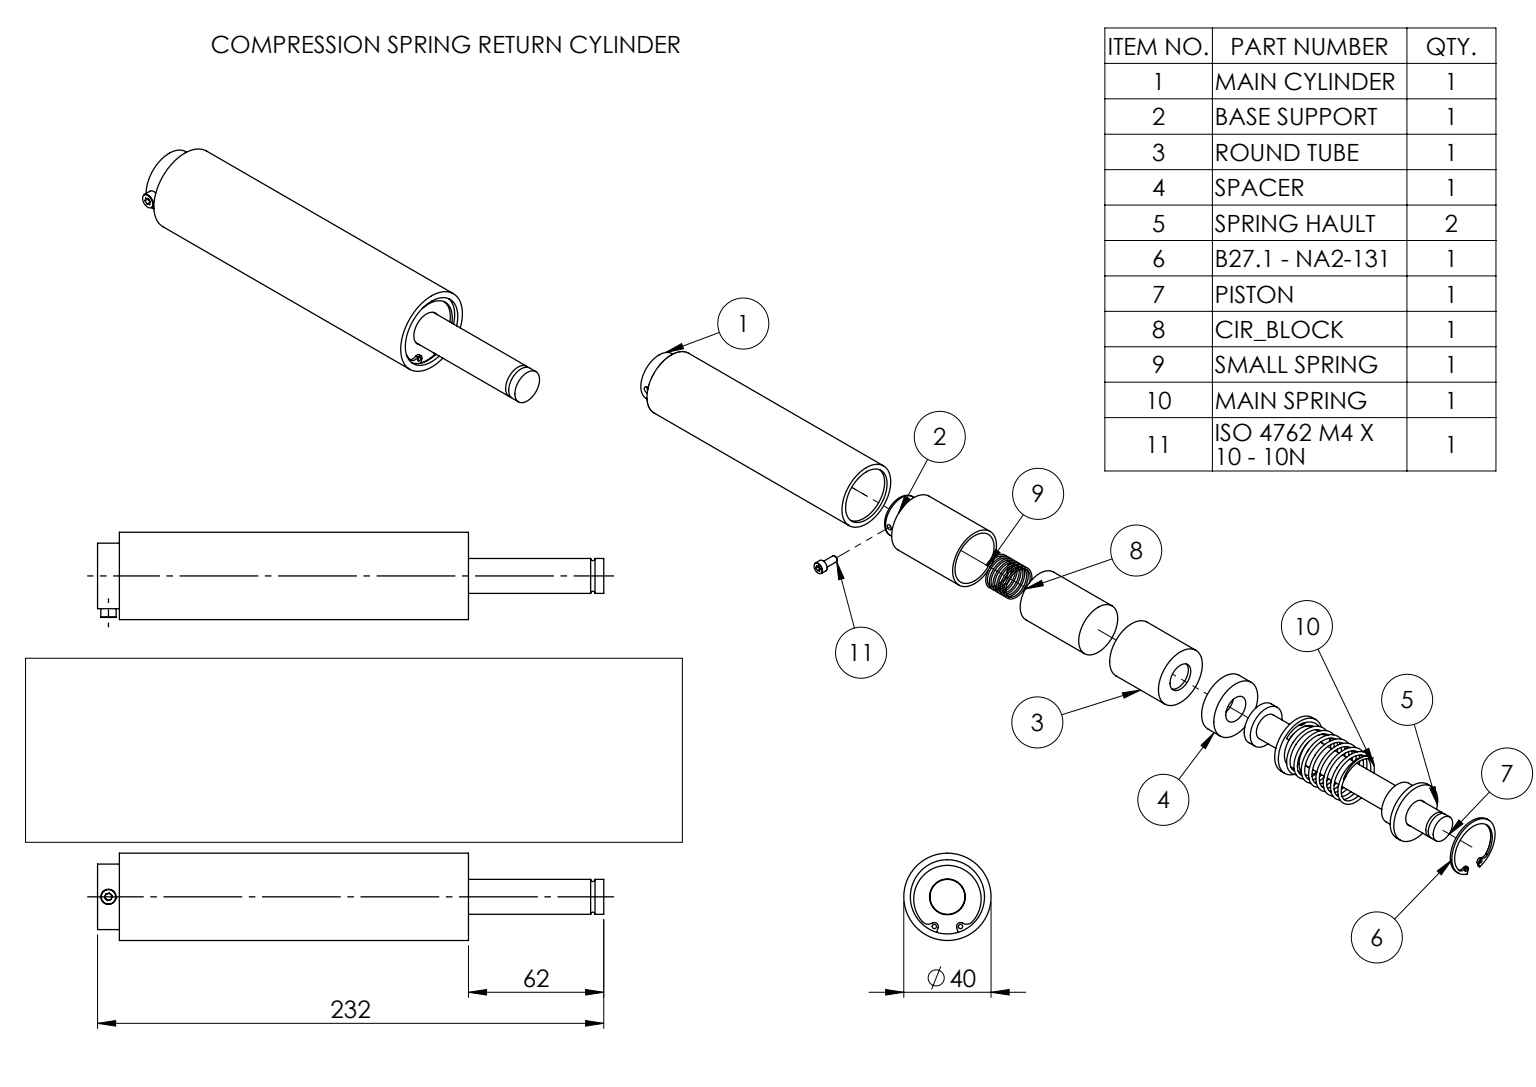
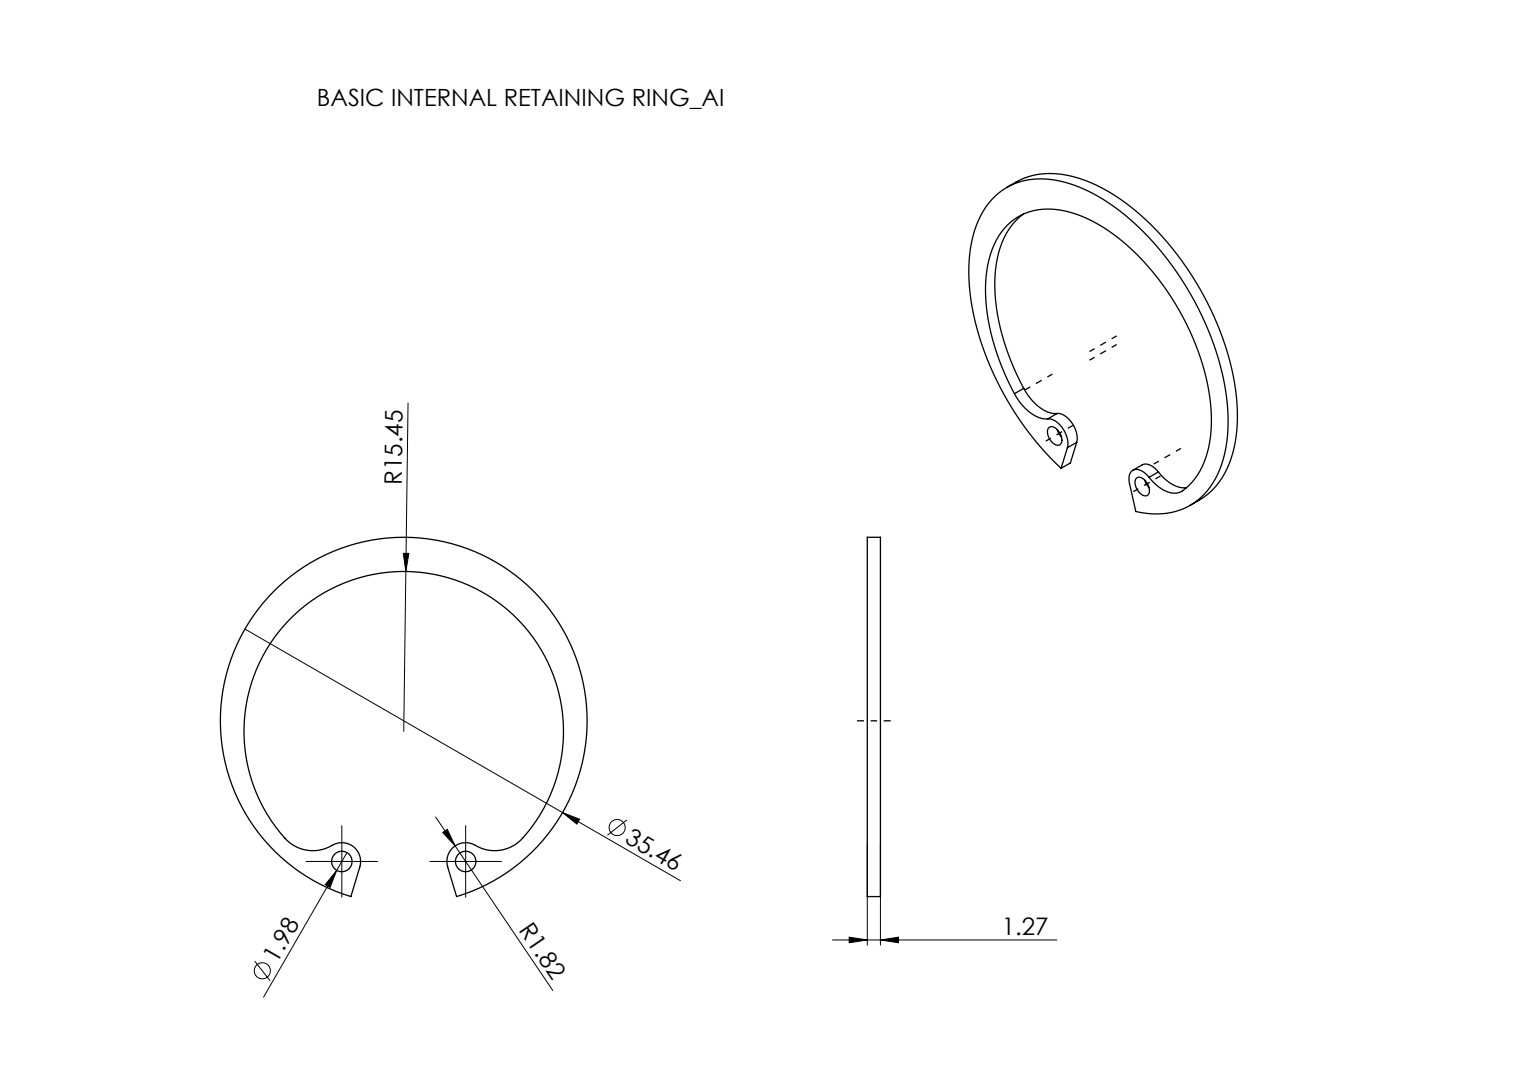
ISO-10303-21;
HEADER;
FILE_DESCRIPTION (('STEP AP214'),
    '1' );
FILE_NAME ('BR-105',
    '2026-10-08T13:22:57',
    ( '' ),
    ( '' ),
    'SwSTEP 2.0',
    'SolidWorks 2026',
    '' );
FILE_SCHEMA (( 'AUTOMOTIVE_DESIGN' ));
ENDSEC;

DATA;
#1 = CARTESIAN_POINT ( 'NONE',  ( -9.837026868206070418, 5.012215536711416952, 5.849999999999989875 ) ) ;
#2 = CARTESIAN_POINT ( 'NONE',  ( 8.512513224245308763, 13.54758718765259040, 13.28571428571429003 ) ) ;
#3 = EDGE_CURVE ( 'NONE', #2841, #2214, #7627, .T. ) ;
#4 = CARTESIAN_POINT ( 'NONE',  ( 0.000000000000000000, 0.000000000000000000, -1.270000000000007123 ) ) ;
#5 = CARTESIAN_POINT ( 'NONE',  ( -14.28433602490915000, 1.478298951650542481, 25.35310228751642470 ) ) ;
#6 = CARTESIAN_POINT ( 'NONE',  ( 9.377220287599001836, 4.724406229267489543, 5.901137918078571687 ) ) ;
#7 = CARTESIAN_POINT ( 'NONE',  ( 8.486213763410640709, 4.270415729527937465, 17.90113791807857524 ) ) ;
#8 = AXIS2_PLACEMENT_3D ( 'NONE', #6315, #4531, #6166 ) ;
#9 = AXIS2_PLACEMENT_3D ( 'NONE', #1726, #4047, #111 ) ;
#10 = LINE ( 'NONE', #4146, #4138 ) ;
#11 = CARTESIAN_POINT ( 'NONE',  ( -11.92174236212692051, -7.340858601238089420, 8.718326283912148256 ) ) ;
#12 = CARTESIAN_POINT ( 'NONE',  ( 13.17239914596754424, -4.743843029824685864, 18.57546914105500235 ) ) ;
#13 = EDGE_CURVE ( 'NONE', #5655, #2841, #6772, .T. ) ;
#14 = ORIENTED_EDGE ( 'NONE', *, *, #6088, .F. ) ;
#15 = CARTESIAN_POINT ( 'NONE',  ( 15.44746603149413922, 5.543385399275817527, 15.92453085894499409 ) ) ;
#16 = COLOUR_RGB ( '', 0.40784314, 0.44705882, 0.49803922) ;
#17 = DIRECTION ( 'NONE',  ( 0.000000000000000000, 0.000000000000000000, 1.000000000000000000 ) ) ;
#18 = AXIS2_PLACEMENT_3D ( 'NONE', #9607, #4018, #5606 ) ;
#19 = AXIS2_PLACEMENT_3D ( 'NONE', #2999, #9984, #6972 ) ;
#20 = CARTESIAN_POINT ( 'NONE',  ( 11.31370849898482334, -11.31370849898469366, 45.00000000000000711 ) ) ;
#21 = CARTESIAN_POINT ( 'NONE',  ( -170.0000000000000284, -1.448262861947153525E-15, 0.000000000000000000 ) ) ;
#22 = CARTESIAN_POINT ( 'NONE',  ( 15.44569104238500046, -1.018491042385001544, -1.270000000000007123 ) ) ;
#23 = CARTESIAN_POINT ( 'NONE',  ( -4.312909747525649706, -8.464561979789507973, 14.10000000000000142 ) ) ;
#24 = CARTESIAN_POINT ( 'NONE',  ( 4.534861676072320158, -8.900167166472098046, 4.650000000000026112 ) ) ;
#25 = CARTESIAN_POINT ( 'NONE',  ( -8.731428362939189114, 13.89598863503036341, 36.21428571428573662 ) ) ;
#26 = CARTESIAN_POINT ( 'NONE',  ( 2.000000000000001776, 0.000000000000000000, 0.000000000000000000 ) ) ;
#27 = LINE ( 'NONE', #8664, #6923 ) ;
#28 = CARTESIAN_POINT ( 'NONE',  ( -11.22385875690717327, 11.40355824106234550, 28.00404056962643651 ) ) ;
#29 = ORIENTED_EDGE ( 'NONE', *, *, #8994, .F. ) ;
#30 = CARTESIAN_POINT ( 'NONE',  ( -1.837501619626328297, 16.30827793483733856, 12.64285714285714235 ) ) ;
#31 = CARTESIAN_POINT ( 'NONE',  ( 0.000000000000000000, -6.162975822039154730E-30, 20.00000000000001776 ) ) ;
#32 = AXIS2_PLACEMENT_3D ( 'NONE', #6124, #2105, #1276 ) ;
#33 = CARTESIAN_POINT ( 'NONE',  ( 0.000000000000000000, 0.000000000000000000, 0.000000000000000000 ) ) ;
#34 = CARTESIAN_POINT ( 'NONE',  ( -7.458344646081709328, 7.390897758835804687, 9.998862081921425116 ) ) ;
#35 = CARTESIAN_POINT ( 'NONE',  ( -13.92619789766827054, -1.441234910513399470, 45.14689771248358596 ) ) ;
#36 = CARTESIAN_POINT ( 'NONE',  ( 8.512513224245308763, 13.54758718765259040, 19.28571428571428825 ) ) ;
#37 = CONTEXT_DEPENDENT_SHAPE_REPRESENTATION ( #2747, #7395 ) ;
#38 = CARTESIAN_POINT ( 'NONE',  ( -7.639999817571786700, 12.15899005565156266, 36.21428571428572951 ) ) ;
#39 = CARTESIAN_POINT ( 'NONE',  ( 9.809645194534072132, -9.989344678689256796, 31.00404056962644006 ) ) ;
#40 = CARTESIAN_POINT ( 'NONE',  ( -9.865911304835474738, -1.562606840307925848, 8.549999999999963407 ) ) ;
#41 = CARTESIAN_POINT ( 'NONE',  ( 5.012215536711511987, -9.837026868205999364, 13.65000000000003233 ) ) ;
#42 = ORIENTED_EDGE ( 'NONE', *, *, #8056, .T. ) ;
#43 = CARTESIAN_POINT ( 'NONE',  ( 1.441234910513245149, 13.92619789766829008, 50.85310228751642825 ) ) ;
#44 = ORIENTED_EDGE ( 'NONE', *, *, #5565, .F. ) ;
#45 = DIRECTION ( 'NONE',  ( 1.000000000000000000, 0.000000000000000000, 0.000000000000000000 ) ) ;
#46 = CARTESIAN_POINT ( 'NONE',  ( 11.60466159355861926, 11.60466159355874716, 13.50000000000000355 ) ) ;
#47 = CIRCLE ( 'NONE', #69, 13.00000000000001066 ) ;
#48 = CARTESIAN_POINT ( 'NONE',  ( -13.96533075980324234, 8.621071003556515677, 19.78167371608784819 ) ) ;
#49 = DIRECTION ( 'NONE',  ( -1.000000000000000000, 0.000000000000000000, -0.000000000000000000 ) ) ;
#50 = CARTESIAN_POINT ( 'NONE',  ( 10.90442828429183919, 1.727091770866679532, 1.049999999999966738 ) ) ;
#51 = CARTESIAN_POINT ( 'NONE',  ( 17.72919999999999874, 0.000000000000000000, -1.270000000000007123 ) ) ;
#52 = CIRCLE ( 'NONE', #2688, 13.00000000000000000 ) ;
#53 = FILL_AREA_STYLE_COLOUR ( '', #3926 ) ;
#54 = EDGE_LOOP ( 'NONE', ( #8916, #8035, #5862, #4936 ) ) ;
#55 = CARTESIAN_POINT ( 'NONE',  ( 4.766900247265192903, 9.355568503977902850, 12.59999999999999964 ) ) ;
#56 = CARTESIAN_POINT ( 'NONE',  ( 1.791431617652837316, 15.89939535829188877, 12.85714285714285943 ) ) ;
#57 = CARTESIAN_POINT ( 'NONE',  ( 0.000000000000000000, 1.773042676681366281, 0.000000000000000000 ) ) ;
#58 = SHAPE_REPRESENTATION ( 'BR-105', ( #5082, #2288, #1626, #7233, #8720, #5896, #6061, #2114, #799, #7563, #6712, #8058, #5576 ), #3109 ) ;
#59 = CARTESIAN_POINT ( 'NONE',  ( 1.441234910513245149, 13.92619789766829008, 26.85310228751642470 ) ) ;
#60 = CARTESIAN_POINT ( 'NONE',  ( 4.809394265263009061, 9.333916720356739916, 8.601137918078563871 ) ) ;
#61 = CARTESIAN_POINT ( 'NONE',  ( -9.873755945037078874, -1.513077731353019706, 10.55113791807857204 ) ) ;
#62 = CARTESIAN_POINT ( 'NONE',  ( -108.0000000000000284, 0.000000000000000000, 18.00000000000000000 ) ) ;
#63 = CARTESIAN_POINT ( 'NONE',  ( 13.17239914596754424, -4.743843029824685864, 12.57546914105500768 ) ) ;
#64 = CARTESIAN_POINT ( 'NONE',  ( -1.478298951650703019, 14.28433602490913579, 10.64689771248357886 ) ) ;
#65 = ORIENTED_EDGE ( 'NONE', *, *, #5817, .F. ) ;
#66 = DIRECTION ( 'NONE',  ( 1.000000000000000000, 4.755747939841215952E-17, -0.000000000000000000 ) ) ;
#67 = ADVANCED_BREP_SHAPE_REPRESENTATION ( '', ( #183, #3995 ), #2439 ) ;
#68 = CARTESIAN_POINT ( 'NONE',  ( 15.89939535829187278, 1.791431617653015174, 44.14285714285714590 ) ) ;
#69 = AXIS2_PLACEMENT_3D ( 'NONE', #6608, #9795, #2698 ) ;
#70 = DIRECTION ( 'NONE',  ( 0.000000000000000000, 0.000000000000000000, 1.000000000000000000 ) ) ;
#71 = FACE_OUTER_BOUND ( 'NONE', #2223, .T. ) ;
#72 = CARTESIAN_POINT ( 'NONE',  ( 9.865911304835474738, 1.562606840307950051, 19.04999999999997939 ) ) ;
#73 = CARTESIAN_POINT ( 'NONE',  ( 8.900167166472154889, -4.534861676072210912, 7.350000000000000533 ) ) ;
#74 = EDGE_CURVE ( 'NONE', #951, #9116, #2667, .T. ) ;
#75 = CARTESIAN_POINT ( 'NONE',  ( -163.1352118936811451, 1.079191317860220156, 12.95565487998667820 ) ) ;
#76 = DIRECTION ( 'NONE',  ( 0.000000000000000000, 8.191099868251446680E-34, 1.000000000000000000 ) ) ;
#77 = CARTESIAN_POINT ( 'NONE',  ( -5.543385399275643444, -15.44746603149420494, 38.07546914105502367 ) ) ;
#78 = ORIENTED_EDGE ( 'NONE', *, *, #9774, .F. ) ;
#79 = CARTESIAN_POINT ( 'NONE',  ( -13.54758718765249625, -8.512513224245459753, 34.71428571428571530 ) ) ;
#80 = CARTESIAN_POINT ( 'NONE',  ( 2.336471713481377055, 15.82515143223400145, 48.73000000000002530 ) ) ;
#81 = DIRECTION ( 'NONE',  ( -4.755747939841216568E-17, 1.000000000000000000, 0.000000000000000000 ) ) ;
#82 = SURFACE_STYLE_USAGE ( .BOTH. , #1640 ) ;
#83 = CARTESIAN_POINT ( 'NONE',  ( 4.724406229267374968, 9.377220287599055126, 13.59886208192140167 ) ) ;
#84 = CARTESIAN_POINT ( 'NONE',  ( 5.056896391392317724, -9.814260835640977731, 14.64886208192141659 ) ) ;
#85 = CARTESIAN_POINT ( 'NONE',  ( -1.693770420379220099, -13.89774397934251837, 43.86118342676930126 ) ) ;
#86 = CARTESIAN_POINT ( 'NONE',  ( 16.30827793483735633, -1.837501619626142890, 20.35714285714286476 ) ) ;
#87 = CARTESIAN_POINT ( 'NONE',  ( -4.742819248065500481, -13.55419868402813499, 34.07142857142857650 ) ) ;
#88 = CARTESIAN_POINT ( 'NONE',  ( -5.164528828830334817, 15.14410076328347543, -1.567388001802134223 ) ) ;
#89 = CARTESIAN_POINT ( 'NONE',  ( -14.26974319298268767, 1.607813917172874918, 5.357142857142856762 ) ) ;
#90 = CARTESIAN_POINT ( 'NONE',  ( -1.486127417882243895, 9.383039235653816590, 15.29999999999997939 ) ) ;
#91 = CARTESIAN_POINT ( 'NONE',  ( 1.727091770866550968, 10.90442828429186761, 18.44999999999999218 ) ) ;
#92 = ORIENTED_EDGE ( 'NONE', *, *, #7588, .T. ) ;
#93 = CARTESIAN_POINT ( 'NONE',  ( -11.85413878919593422, -7.448449071214776396, 4.714285714285712636 ) ) ;
#94 = VERTEX_POINT ( 'NONE', #2924 ) ;
#95 = DIRECTION ( 'NONE',  ( 0.000000000000000000, 0.000000000000000000, 1.000000000000000000 ) ) ;
#96 = CARTESIAN_POINT ( 'NONE',  ( -8.512513224245306986, -13.54758718765259218, 16.28571428571428470 ) ) ;
#97 = CARTESIAN_POINT ( 'NONE',  ( -16.32287076676382398, 1.707986654103809343, 43.35310228751642825 ) ) ;
#98 = CARTESIAN_POINT ( 'NONE',  ( -160.0000000000000284, 19.99999999999999289, 0.000000000000000000 ) ) ;
#99 = CARTESIAN_POINT ( 'NONE',  ( -7.806708723663830618, -7.806708723663906113, 8.250000000000028422 ) ) ;
#100 = EDGE_CURVE ( 'NONE', #8895, #4771, #529, .T. ) ;
#101 = CARTESIAN_POINT ( 'NONE',  ( 4.742819248065502258, 13.55419868402813499, 1.071428571428570065 ) ) ;
#102 =( LENGTH_UNIT ( ) NAMED_UNIT ( * ) SI_UNIT ( .MILLI., .METRE. ) );
#103 = EDGE_LOOP ( 'NONE', ( #4875, #2005 ) ) ;
#104 = CARTESIAN_POINT ( 'NONE',  ( -10.06191849875405531, -10.24623928997363542, 12.49595943037356349 ) ) ;
#105 = CARTESIAN_POINT ( 'NONE',  ( -5.012215536711508435, 9.837026868206029562, 9.150000000000002132 ) ) ;
#106 = CARTESIAN_POINT ( 'NONE',  ( -163.3500000000000796, 0.1091377801384209867, 13.00000000000000178 ) ) ;
#107 = CARTESIAN_POINT ( 'NONE',  ( 7.750357176954296712, -12.08964793087877787, 41.21024514465928235 ) ) ;
#108 = CARTESIAN_POINT ( 'NONE',  ( -10.91227292449344155, -1.677562661911748965, 4.551137918078585365 ) ) ;
#109 = CARTESIAN_POINT ( 'NONE',  ( 9.375578539472099848, -1.533232399699987702, 15.20113791807854575 ) ) ;
#110 = CIRCLE ( 'NONE', #5390, 0.2000000000000000944 ) ;
#111 = DIRECTION ( 'NONE',  ( 1.000000000000000000, 0.000000000000000000, 0.000000000000000000 ) ) ;
#112 = CARTESIAN_POINT ( 'NONE',  ( -7.556039541191334585, -11.78653521626503320, 2.289754855340722539 ) ) ;
#113 =( LENGTH_UNIT ( ) NAMED_UNIT ( * ) SI_UNIT ( .MILLI., .METRE. ) );
#114 = CARTESIAN_POINT ( 'NONE',  ( 7.556039541191335474, 11.78653521626503320, 11.28975485534071943 ) ) ;
#115 = ORIENTED_EDGE ( 'NONE', *, *, #1311, .F. ) ;
#117 = CARTESIAN_POINT ( 'NONE',  ( 0.2000000000000057288, 4.041334437186265510E-16, -3.299999999999999822 ) ) ;
#116 = STYLED_ITEM ( 'NONE', ( #9052 ), #3700 ) ;
#118 = CARTESIAN_POINT ( 'NONE',  ( 11.60466159355862104, 11.60466159355875071, 37.50000000000002842 ) ) ;
#119 = CYLINDRICAL_SURFACE ( 'NONE', #383, 0.9906000000000003691 ) ;
#120 = CARTESIAN_POINT ( 'NONE',  ( -167.0926989554971556, -0.5670040589733402747, 14.99151548021192148 ) ) ;
#121 = CARTESIAN_POINT ( 'NONE',  ( 1.562606840307832368, 9.865911304835503159, 18.44999999999999218 ) ) ;
#122 = CARTESIAN_POINT ( 'NONE',  ( 7.063212654743467489, 7.063212654743559860, 3.749999999999997335 ) ) ;
#123 = CARTESIAN_POINT ( 'NONE',  ( -166.9317395015584680, 0.9543248124665052456, 12.96558013998003922 ) ) ;
#124 = CARTESIAN_POINT ( 'NONE',  ( 16.29368510291089223, -1.967016585148476882, 30.36118342676929771 ) ) ;
#125 = CARTESIAN_POINT ( 'NONE',  ( 7.063212654743468377, 7.063212654743558083, 0.7499999999999762412 ) ) ;
#126 = CARTESIAN_POINT ( 'NONE',  ( -11.22385875690717327, 11.40355824106234550, 34.00404056962644006 ) ) ;
#127 = EDGE_LOOP ( 'NONE', ( #6964, #4432, #9166, #5764, #3012, #4282, #881, #9298, #4822, #5247, #5054, #1752, #8600 ) ) ;
#128 = CARTESIAN_POINT ( 'NONE',  ( 8.731428362939190890, -13.89598863503036164, 33.21428571428571530 ) ) ;
#129 = CARTESIAN_POINT ( 'NONE',  ( 2.000000000000001776, 0.8865213383406900238, 1.535499999999967446 ) ) ;
#130 = CARTESIAN_POINT ( 'NONE',  ( 11.60466159355862104, 11.60466159355875071, 1.500000000000003553 ) ) ;
#131 = SURFACE_STYLE_FILL_AREA ( #8771 ) ;
#132 = ADVANCED_FACE ( 'NONE', ( #2160 ), #9918, .F. ) ;
#133 =( NAMED_UNIT ( * ) PLANE_ANGLE_UNIT ( ) SI_UNIT ( $, .RADIAN. ) );
#134 = CARTESIAN_POINT ( 'NONE',  ( -8.442910196168309511, -4.355403765523546689, 6.398862081921404155 ) ) ;
#135 = CARTESIAN_POINT ( 'NONE',  ( -5.056896391392315948, 9.814260835640997271, 16.14886208192145389 ) ) ;
#136 = CARTESIAN_POINT ( 'NONE',  ( 5.164528828830335705, -15.14410076328347543, 1.432611998197868219 ) ) ;
#137 = CARTESIAN_POINT ( 'NONE',  ( -1.791431617652833763, -15.89939535829188877, 21.85714285714286120 ) ) ;
#138 = CARTESIAN_POINT ( 'NONE',  ( -11.85413878919593422, -7.448449071214776396, 34.71428571428571530 ) ) ;
#139 = CARTESIAN_POINT ( 'NONE',  ( -9.809645194534070356, 9.989344678689256796, 46.00404056962644006 ) ) ;
#140 = CARTESIAN_POINT ( 'NONE',  ( -7.639999817571787588, 12.15899005565156266, 12.21428571428571885 ) ) ;
#141 = CARTESIAN_POINT ( 'NONE',  ( 1.562606840307832146, 9.865911304835508489, 15.44999999999997797 ) ) ;
#142 = CARTESIAN_POINT ( 'NONE',  ( -9.333916720356675967, -4.809394265263095214, 12.39886208192140948 ) ) ;
#143 = ORIENTED_EDGE ( 'NONE', *, *, #7111, .T. ) ;
#144 = CARTESIAN_POINT ( 'NONE',  ( -11.78653521626494793, -7.556039541191465148, 48.71024514465926814 ) ) ;
#145 = EDGE_LOOP ( 'NONE', ( #8443, #9716, #3991, #7695 ) ) ;
#146 = CARTESIAN_POINT ( 'NONE',  ( 0.000000000000000000, 0.8865213383407039016, -1.535500000000022958 ) ) ;
#147 = MANIFOLD_SOLID_BREP ( 'Revolve1', #1849 ) ;
#148 = CARTESIAN_POINT ( 'NONE',  ( 1.791431617652837316, 15.89939535829188877, 18.85714285714285765 ) ) ;
#149 = CARTESIAN_POINT ( 'NONE',  ( -15.14410076328353227, 5.164528828830164287, 31.56738800180213644 ) ) ;
#150 = CARTESIAN_POINT ( 'NONE',  ( -4.766900247265192014, -9.355568503977867323, 8.099999999999996092 ) ) ;
#151 = CARTESIAN_POINT ( 'NONE',  ( -4.766900247265192014, -9.355568503977867323, 8.099999999999996092 ) ) ;
#152 = FACE_BOUND ( 'NONE', #612, .T. ) ;
#153 = FILL_AREA_STYLE ('',( #53 ) ) ;
#154 = ORIENTED_EDGE ( 'NONE', *, *, #7460, .T. ) ;
#155 = CARTESIAN_POINT ( 'NONE',  ( -1.441234910513241818, -13.92619789766829008, 11.85310228751642470 ) ) ;
#156 = CARTESIAN_POINT ( 'NONE',  ( -5.012215536711508435, 9.837026868206020680, 18.15000000000000924 ) ) ;
#157 = CARTESIAN_POINT ( 'NONE',  ( -58.00000000000002842, 7.703719777548943412E-30, -1.059261469412979719E-30 ) ) ;
#158 = CARTESIAN_POINT ( 'NONE',  ( 7.340858601237956194, 11.92174236212700045, 45.28167371608785174 ) ) ;
#159 = CARTESIAN_POINT ( 'NONE',  ( -4.967534682030703586, 9.859792900771061852, 17.15113791807853616 ) ) ;
#160 = CARTESIAN_POINT ( 'NONE',  ( 4.490180821391514421, -8.922933199037132113, 12.65113791807859123 ) ) ;
#161 = EDGE_CURVE ( 'NONE', #3385, #4901, #5306, .T. ) ;
#162 = DIRECTION ( 'NONE',  ( 1.000000000000000000, 0.000000000000000000, 0.000000000000000000 ) ) ;
#163 = CARTESIAN_POINT ( 'NONE',  ( 4.865839792409144771, 13.51115193377589740, 17.07546914105500591 ) ) ;
#164 = AXIS2_PLACEMENT_3D ( 'NONE', #7046, #7979, #7201 ) ;
#165 = CARTESIAN_POINT ( 'NONE',  ( -11.92174236212692051, -7.340858601238089420, 8.718326283912148256 ) ) ;
#166 = VERTEX_POINT ( 'NONE', #3235 ) ;
#167 = LINE ( 'NONE', #8073, #9856 ) ;
#168 = CARTESIAN_POINT ( 'NONE',  ( -5.404401153735176599, 15.06016580658422477, 14.42453085894499232 ) ) ;
#169 = CYLINDRICAL_SURFACE ( 'NONE', #4836, 18.00000000000002132 ) ;
#170 = CARTESIAN_POINT ( 'NONE',  ( -165.9524913265358350, -1.932636693197999911, 14.87507538773749438 ) ) ;
#171 = CIRCLE ( 'NONE', #2486, 11.00000000000000355 ) ;
#172 = TOROIDAL_SURFACE ( 'NONE', #9093, 2.200000000000001066, 0.2000000000000000111 ) ;
#173 = CARTESIAN_POINT ( 'NONE',  ( -1.439022436064386845, 9.390499931835535108, 8.301137918078554279 ) ) ;
#174 = CARTESIAN_POINT ( 'NONE',  ( 1.486127417882244783, -9.383039235653782839, 7.800000000000029132 ) ) ;
#175 = CARTESIAN_POINT ( 'NONE',  ( -166.3219090446497432, 1.718560695228406932, 12.88744630017030168 ) ) ;
#176 = CARTESIAN_POINT ( 'NONE',  ( 8.621071003556677326, -13.96533075980314287, 31.21832628391215536 ) ) ;
#177 = CARTESIAN_POINT ( 'NONE',  ( -4.312909747525649706, -8.464561979789507973, 2.099999999999990763 ) ) ;
#178 = ADVANCED_FACE ( 'NONE', ( #1639 ), #6426, .T. ) ;
#179 = CARTESIAN_POINT ( 'NONE',  ( 8.620103694221997515, 13.47998361472160767, 29.28975485534071765 ) ) ;
#180 = CIRCLE ( 'NONE', #1825, 18.00000000000002132 ) ;
#181 = CIRCLE ( 'NONE', #5941, 18.00000000000000355 ) ;
#182 = ORIENTED_EDGE ( 'NONE', *, *, #837, .T. ) ;
#183 = MANIFOLD_SOLID_BREP ( 'Hex', #8118 ) ;
#184 = CARTESIAN_POINT ( 'NONE',  ( -15.89939535829186923, -1.791431617653016062, 29.14285714285714235 ) ) ;
#185 = CARTESIAN_POINT ( 'NONE',  ( -1.732852372895761661, 14.17511762181074353, 2.529641460854714575E-15 ) ) ;
#186 = CARTESIAN_POINT ( 'NONE',  ( -5.420364854931999155, -15.49051278174644253, 22.07142857142858006 ) ) ;
#187 =( NAMED_UNIT ( * ) PLANE_ANGLE_UNIT ( ) SI_UNIT ( $, .RADIAN. ) );
#188 = CARTESIAN_POINT ( 'NONE',  ( 5.986002070941135678, -13.58603705635637304, -1.270000000000007123 ) ) ;
#189 = AXIS2_PLACEMENT_3D ( 'NONE', #6209, #7825, #5544 ) ;
#190 = CARTESIAN_POINT ( 'NONE',  ( -9.390499931835536884, 1.439022436064298249, 6.698862081921455491 ) ) ;
#191 = CARTESIAN_POINT ( 'NONE',  ( -1.533232399700100057, 9.375578539472094519, 1.298862081921425604 ) ) ;
#192 =( GEOMETRIC_REPRESENTATION_CONTEXT ( 3 ) GLOBAL_UNCERTAINTY_ASSIGNED_CONTEXT ( ( #920 ) ) GLOBAL_UNIT_ASSIGNED_CONTEXT ( ( #9393, #2545, #4632 ) ) REPRESENTATION_CONTEXT ( 'NONE', 'WORKASPACE' ) );
#193 = UNCERTAINTY_MEASURE_WITH_UNIT (LENGTH_MEASURE( 1.000000000000000082E-05 ), #7498, 'distance_accuracy_value', 'NONE');
#194 = CARTESIAN_POINT ( 'NONE',  ( 12.08964793087886314, -7.750357176954162597, 42.78975485534072476 ) ) ;
#195 = CARTESIAN_POINT ( 'NONE',  ( 8.731428362939190890, -13.89598863503036164, 9.214285714285717077 ) ) ;
#196 = DIRECTION ( 'NONE',  ( 1.000000000000000000, 0.000000000000000000, 0.000000000000000000 ) ) ;
#197 = CARTESIAN_POINT ( 'NONE',  ( 4.503970704919991519, -13.25633410266674517, 43.43261199819787066 ) ) ;
#198 = CARTESIAN_POINT ( 'NONE',  ( -1.567502665446231180, -13.91197093850540334, 9.857142857142855874 ) ) ;
#199 = CARTESIAN_POINT ( 'NONE',  ( -4.534861676072319270, 8.900167166472117586, 18.15000000000000924 ) ) ;
#200 = CARTESIAN_POINT ( 'NONE',  ( -9.333916720356675967, -4.809394265263096990, 9.398862081921446787 ) ) ;
#201 = ORIENTED_EDGE ( 'NONE', *, *, #7622, .F. ) ;
#202 = CARTESIAN_POINT ( 'NONE',  ( 4.742819248065503146, 13.55419868402813677, 7.071428571428569398 ) ) ;
#203 = VECTOR ( 'NONE', #8292, 1000.000000000000000 ) ;
#204 = ORIENTED_EDGE ( 'NONE', *, *, #7487, .T. ) ;
#205 = CARTESIAN_POINT ( 'NONE',  ( -9.899494936611716867, 9.899494936611610285, 0.000000000000000000 ) ) ;
#206 = MANIFOLD_SOLID_BREP ( 'Sweep1', #9455 ) ;
#207 = CARTESIAN_POINT ( 'NONE',  ( 15.10213328493390783, -5.284464991282587398, 14.57142857142856940 ) ) ;
#208 = CARTESIAN_POINT ( 'NONE',  ( 5.404401153735178376, -15.06016580658422477, 35.42453085894499765 ) ) ;
#209 = CARTESIAN_POINT ( 'NONE',  ( -10.37072757624895836, 1.642561882922381145, 5.700000000000038369 ) ) ;
#210 = CARTESIAN_POINT ( 'NONE',  ( 5.012215536711511987, -9.837026868205999364, 13.65000000000003233 ) ) ;
#211 = ADVANCED_FACE ( 'NONE', ( #9553 ), #5041, .F. ) ;
#212 = DIRECTION ( 'NONE',  ( 0.000000000000000000, -1.224646799147353454E-16, 1.000000000000000000 ) ) ;
#213 = CARTESIAN_POINT ( 'NONE',  ( 1.727091770866551412, 10.90442828429187117, 15.44999999999997797 ) ) ;
#214 = CARTESIAN_POINT ( 'NONE',  ( -163.5173699842553390, 0.7321227054117522837, 12.97975339917165805 ) ) ;
#215 = CARTESIAN_POINT ( 'NONE',  ( 4.743843029824831525, -13.17239914596749095, 41.42453085894499765 ) ) ;
#216 = CARTESIAN_POINT ( 'NONE',  ( 9.377220287599001836, 4.724406229267489543, 14.90113791807857879 ) ) ;
#217 = CARTESIAN_POINT ( 'NONE',  ( -8.877401133907129704, 4.579542530753042406, 13.85113791807855321 ) ) ;
#218 = DIRECTION ( 'NONE',  ( 0.000000000000000000, -6.338944243255235518E-49, 1.000000000000000000 ) ) ;
#219 = CARTESIAN_POINT ( 'NONE',  ( -4.503970704919988854, 13.25633410266674517, 22.43261199819786356 ) ) ;
#220 = CARTESIAN_POINT ( 'NONE',  ( -13.92619789766827054, -1.441234910513399470, 15.14689771248357708 ) ) ;
#221 = EDGE_LOOP ( 'NONE', ( #1092, #6507, #3813, #5099, #9566 ) ) ;
#222 = CARTESIAN_POINT ( 'NONE',  ( -8.084771497730057628E-16, 16.99999999999997868, 0.000000000000000000 ) ) ;
#223 = CARTESIAN_POINT ( 'NONE',  ( -11.40355824106246807, 11.22385875690704715, 7.995959430373565269 ) ) ;
#224 = LINE ( 'NONE', #5694, #1710 ) ;
#225 = CARTESIAN_POINT ( 'NONE',  ( -164.3051146695663363, -2.039487319166105372, 14.86080315614530534 ) ) ;
#226 = CARTESIAN_POINT ( 'NONE',  ( 7.098671581784200768, 7.027753727702831021, 8.751137918078539357 ) ) ;
#227 = CARTESIAN_POINT ( 'NONE',  ( -8.464561979789474222, -4.312909747525729642, 8.399999999999963052 ) ) ;
#228 = CARTESIAN_POINT ( 'NONE',  ( -164.8603154174794270, 2.150053139255677870, 12.82096999065581322 ) ) ;
#229 = CARTESIAN_POINT ( 'NONE',  ( 1.917699372585825790, 15.88516839912900203, 34.86118342676929416 ) ) ;
#230 = CARTESIAN_POINT ( 'NONE',  ( -14.26974319298268767, 1.607813917172874918, 29.35714285714285765 ) ) ;
#231 = EDGE_CURVE ( 'NONE', #1952, #8798, #6117, .T. ) ;
#232 = CARTESIAN_POINT ( 'NONE',  ( 5.543385399275644332, 15.44746603149420494, 41.07546914105501656 ) ) ;
#233 = ORIENTED_EDGE ( 'NONE', *, *, #6419, .T. ) ;
#234 = AXIS2_PLACEMENT_3D ( 'NONE', #895, #1048, #264 ) ;
#235 = CARTESIAN_POINT ( 'NONE',  ( 1.791431617652837316, 15.89939535829188877, 24.85714285714285765 ) ) ;
#236 = CARTESIAN_POINT ( 'NONE',  ( -0.4153140463578967601, 14.34878908348401971, 2.773985284965652638E-17 ) ) ;
#237 = CARTESIAN_POINT ( 'NONE',  ( -1.837501619626328297, 16.30827793483733856, 18.64285714285715656 ) ) ;
#238 =( NAMED_UNIT ( * ) SI_UNIT ( $, .STERADIAN. ) SOLID_ANGLE_UNIT ( ) );
#239 = DIRECTION ( 'NONE',  ( -4.755747939841215952E-17, 1.000000000000000000, 0.000000000000000000 ) ) ;
#240 = CARTESIAN_POINT ( 'NONE',  ( 8.922933199037192509, -4.490180821391404287, 14.34886208192142831 ) ) ;
#241 = CARTESIAN_POINT ( 'NONE',  ( 11.31370849898482334, -11.31370849898469366, 39.00000000000000000 ) ) ;
#242 = CARTESIAN_POINT ( 'NONE',  ( -10.89658364409024749, -1.776620879821561694, 15.54886208192143293 ) ) ;
#243 = CARTESIAN_POINT ( 'NONE',  ( 15.91362231745475597, 1.665163862720026255, 0.1468977124835755543 ) ) ;
#244 = CARTESIAN_POINT ( 'NONE',  ( 13.54758718765249803, 8.512513224245457977, 31.71428571428571530 ) ) ;
#245 = CARTESIAN_POINT ( 'NONE',  ( 0.000000000000000000, 0.000000000000000000, 0.000000000000000000 ) ) ;
#246 = CARTESIAN_POINT ( 'NONE',  ( 7.529642458189280241, -12.22833218042435099, 43.21832628391217668 ) ) ;
#247 = CARTESIAN_POINT ( 'NONE',  ( -13.91197093850538380, -1.567502665446387278, 17.14285714285713880 ) ) ;
#248 = DIRECTION ( 'NONE',  ( 0.000000000000000000, 6.338944243255235518E-49, -1.000000000000000000 ) ) ;
#249 = CARTESIAN_POINT ( 'NONE',  ( 4.724406229267374968, 9.377220287599060455, 10.59886208192144075 ) ) ;
#250 = ORIENTED_EDGE ( 'NONE', *, *, #8801, .F. ) ;
#251 = CARTESIAN_POINT ( 'NONE',  ( 10.15407889436379030, 10.15407889436390576, 19.50000000000000355 ) ) ;
#252 = ORIENTED_EDGE ( 'NONE', *, *, #5467, .F. ) ;
#253 = CARTESIAN_POINT ( 'NONE',  ( -17.72919999999999874, 2.171200803144325526E-15, 1.376312083204286382E-63 ) ) ;
#254 = MANIFOLD_SOLID_BREP ( 'Revolve-Thin1', #5480 ) ;
#255 = CARTESIAN_POINT ( 'NONE',  ( 5.420364854932000931, 15.49051278174644075, 13.07142857142857117 ) ) ;
#256 = CARTESIAN_POINT ( 'NONE',  ( 1.665163862719847732, 15.91362231745477374, 38.85310228751641404 ) ) ;
#257 = APPLICATION_CONTEXT ( 'automotive_design' ) ;
#258 = CARTESIAN_POINT ( 'NONE',  ( 10.90442828429183919, 1.727091770866679532, 10.05000000000002736 ) ) ;
#259 = CARTESIAN_POINT ( 'NONE',  ( -10.90442828429183919, -1.727091770866654663, 14.55000000000000249 ) ) ;
#260 = CARTESIAN_POINT ( 'NONE',  ( 10.15407889436379030, 10.15407889436390221, 7.500000000000004441 ) ) ;
#261 = EDGE_LOOP ( 'NONE', ( #862, #304 ) ) ;
#262 = CARTESIAN_POINT ( 'NONE',  ( -7.340858601237953529, -11.92174236212700222, 24.28167371608785530 ) ) ;
#263 = CARTESIAN_POINT ( 'NONE',  ( -9.837026868206070418, 5.012215536711416952, 11.84999999999997478 ) ) ;
#264 = DIRECTION ( 'NONE',  ( 0.7071067811865432429, 0.7071067811865519026, 0.000000000000000000 ) ) ;
#265 = CARTESIAN_POINT ( 'NONE',  ( 12.22833218042443271, -7.529642458189144349, 34.78167371608785885 ) ) ;
#266 = CARTESIAN_POINT ( 'NONE',  ( 7.390897758835871301, -7.458344646081617846, 18.50113791807859087 ) ) ;
#267 = CARTESIAN_POINT ( 'NONE',  ( 9.814260835641038128, -5.056896391392200485, 6.351137918078572753 ) ) ;
#268 = EDGE_CURVE ( 'NONE', #3156, #7778, #4308, .T. ) ;
#269 = CARTESIAN_POINT ( 'NONE',  ( 0.000000000000000000, 0.000000000000000000, 0.000000000000000000 ) ) ;
#270 =( NAMED_UNIT ( * ) SI_UNIT ( $, .STERADIAN. ) SOLID_ANGLE_UNIT ( ) );
#271 = CARTESIAN_POINT ( 'NONE',  ( 13.59724543428031573, 4.619798703722006294, 23.93261199819786711 ) ) ;
#272 = CARTESIAN_POINT ( 'NONE',  ( -10.90442828429183919, -1.727091770866655329, 8.549999999999963407 ) ) ;
#273 = VERTEX_POINT ( 'NONE', #6004 ) ;
#274 = DIRECTION ( 'NONE',  ( 0.000000000000000000, 1.000000000000000000, 0.000000000000000000 ) ) ;
#275 = CARTESIAN_POINT ( 'NONE',  ( 15.44746603149413922, 5.543385399275817527, 3.924530858944990541 ) ) ;
#276 = CARTESIAN_POINT ( 'NONE',  ( 0.000000000000000000, -1.018491042385001544, 0.000000000000000000 ) ) ;
#277 = CARTESIAN_POINT ( 'NONE',  ( -164.4415472335243180, -2.080930162503950687, 14.85498226103907626 ) ) ;
#278 = CARTESIAN_POINT ( 'NONE',  ( 8.486213763410640709, 4.270415729527937465, 5.901137918078571687 ) ) ;
#279 = CARTESIAN_POINT ( 'NONE',  ( -4.534861676072319270, 8.900167166472117586, 18.15000000000000924 ) ) ;
#280 = FACE_OUTER_BOUND ( 'NONE', #4887, .T. ) ;
#281 = CARTESIAN_POINT ( 'NONE',  ( -11.22385875690717327, 11.40355824106234550, 34.00404056962644006 ) ) ;
#282 = CARTESIAN_POINT ( 'NONE',  ( -13.55419868402807992, -4.742819248065651472, 34.92857142857145192 ) ) ;
#283 = AXIS2_PLACEMENT_3D ( 'NONE', #9014, #7552, #10191 ) ;
#284 = CARTESIAN_POINT ( 'NONE',  ( -4.742819248065502258, -13.55419868402813677, 34.07142857142859071 ) ) ;
#285 = VERTEX_POINT ( 'NONE', #7734 ) ;
#286 = MANIFOLD_SOLID_BREP ( 'Revolve1', #1357 ) ;
#287 = CARTESIAN_POINT ( 'NONE',  ( -5.420364854931999155, -15.49051278174644253, 28.07142857142857295 ) ) ;
#288 = CARTESIAN_POINT ( 'NONE',  ( -3.668565799300981034, 13.66277435358085235, 2.529641460854714969E-15 ) ) ;
#289 = CARTESIAN_POINT ( 'NONE',  ( -8.512513224245306986, -13.54758718765259218, 10.28571428571428648 ) ) ;
#290 = EDGE_CURVE ( 'NONE', #9194, #8643, #8941, .T. ) ;
#291 = FACE_BOUND ( 'NONE', #7704, .T. ) ;
#292 = CARTESIAN_POINT ( 'NONE',  ( -8.442910196168309511, -4.355403765523546689, 18.39886208192140771 ) ) ;
#293 = CARTESIAN_POINT ( 'NONE',  ( 10.89658364409024749, 1.776620879821585897, 20.04886208192142050 ) ) ;
#294 = CARTESIAN_POINT ( 'NONE',  ( -8.621071003556675549, 13.96533075980314642, 16.21832628391214470 ) ) ;
#295 = CARTESIAN_POINT ( 'NONE',  ( 13.89598863503046111, -8.731428362939032795, 32.78571428571430602 ) ) ;
#296 = ADVANCED_FACE ( 'NONE', ( #9134 ), #1342, .T. ) ;
#297 = DIRECTION ( 'NONE',  ( 1.000000000000000000, 4.755747939841215952E-17, -0.000000000000000000 ) ) ;
#298 = CARTESIAN_POINT ( 'NONE',  ( -5.543385399275643444, -15.44746603149420494, 8.075469141055007682 ) ) ;
#299 = CARTESIAN_POINT ( 'NONE',  ( -14.26974319298268767, 1.607813917172874918, 11.35714285714285943 ) ) ;
#300 = CARTESIAN_POINT ( 'NONE',  ( 4.312909747525650594, 8.464561979789532842, 15.60000000000000320 ) ) ;
#301 = CARTESIAN_POINT ( 'NONE',  ( 1.689666864740335894, -10.36326688006721497, 11.79886208192143471 ) ) ;
#302 = ORIENTED_EDGE ( 'NONE', *, *, #7014, .T. ) ;
#303 = CARTESIAN_POINT ( 'NONE',  ( -10.15407889436378852, -10.15407889436390576, 10.50000000000000533 ) ) ;
#304 = ORIENTED_EDGE ( 'NONE', *, *, #4917, .T. ) ;
#305 = CARTESIAN_POINT ( 'NONE',  ( 15.89939535829187278, 1.791431617653015174, 32.14285714285714590 ) ) ;
#306 = CARTESIAN_POINT ( 'NONE',  ( 11.51250119794888249, 11.69682198916847682, 33.49595943037355994 ) ) ;
#307 = CARTESIAN_POINT ( 'NONE',  ( 1.642561882922480621, -10.37072757624891750, 7.800000000000029132 ) ) ;
#308 = PRODUCT ( 'main cylinder', 'main cylinder', '', ( #3194 ) ) ;
#309 = CARTESIAN_POINT ( 'NONE',  ( -1.567502665446231180, -13.91197093850540334, 9.857142857142855874 ) ) ;
#310 = EDGE_CURVE ( 'NONE', #9116, #951, #8435, .T. ) ;
#311 = ORIENTED_EDGE ( 'NONE', *, *, #4917, .F. ) ;
#312 = CARTESIAN_POINT ( 'NONE',  ( 13.89774397934249706, 1.693770420379375308, 22.13881657323070939 ) ) ;
#313 = EDGE_LOOP ( 'NONE', ( #4589, #4798, #9873, #8476 ) ) ;
#314 = DIRECTION ( 'NONE',  ( 0.000000000000000000, 1.000000000000000000, 0.000000000000000000 ) ) ;
#315 = CARTESIAN_POINT ( 'NONE',  ( 4.743843029824831525, -13.17239914596749095, 35.42453085894499765 ) ) ;
#316 = CARTESIAN_POINT ( 'NONE',  ( -5.012215536711506658, 9.837026868206027785, 0.1499999999999952482 ) ) ;
#317 = CARTESIAN_POINT ( 'NONE',  ( 7.842167650704563897, 7.771249796623202144, 8.751137918078539357 ) ) ;
#318 = LINE ( 'NONE', #5785, #2654 ) ;
#319 = CARTESIAN_POINT ( 'NONE',  ( 1.727091770866550968, 10.90442828429187294, 3.450000000000006839 ) ) ;
#320 = CARTESIAN_POINT ( 'NONE',  ( -11.40355824106246807, 11.22385875690704715, 43.99595943037355994 ) ) ;
#321 = ORIENTED_EDGE ( 'NONE', *, *, #2438, .F. ) ;
#322 = CARTESIAN_POINT ( 'NONE',  ( -12.95959046474881227, 7.269551181504937176, 48.73000000000000398 ) ) ;
#323 = CARTESIAN_POINT ( 'NONE',  ( 15.89939535829187278, 1.791431617653015174, 20.14285714285714235 ) ) ;
#324 = CARTESIAN_POINT ( 'NONE',  ( 16.32287076676382043, -1.707986654103810897, 16.35310228751641759 ) ) ;
#325 = CARTESIAN_POINT ( 'NONE',  ( -165.4284909017565326, -1.597016366731424553, 12.90154986763612577 ) ) ;
#326 = CARTESIAN_POINT ( 'NONE',  ( -164.0447505768503618, -1.931287831231678132, 14.87525146959452371 ) ) ;
#327 = CARTESIAN_POINT ( 'NONE',  ( 8.877401133907127928, -4.579542530753017537, 9.351137918078563871 ) ) ;
#329 = VECTOR ( 'NONE', #7005, 1000.000000000000000 ) ;
#328 = CARTESIAN_POINT ( 'NONE',  ( 8.464561979789474222, 4.312909747525755400, 18.90000000000002700 ) ) ;
#330 =( BOUNDED_CURVE ( )  B_SPLINE_CURVE ( 2, ( #1514, #9215, #5487, #10036, #7667, #6246, #5333, #2234, #7861, #8431, #2948, #2187, #6092, #786, #3003, #6917, #1413, #3937, #8645, #6864, #4564, #3053, #741, #637, #9270, #3888, #10090, #7717, #2284, #1567, #6978, #5381, #8538, #4713, #7080, #3840, #3106, #6146, #10139, #1, #1463, #8488, #7032, #7766, #692, #1358, #583, #3729, #6197, #9372, #5429, #8589, #4663, #2129, #7814, #3158, #5271, #4512, #3992, #5682, #3258, #105, #8116, #4813, #4914, #7237, #6452, #5534, #6297, #8061, #7909, #3313, #4967, #989, #9631, #2434, #8693, #8897, #4042, #263, #9481, #942, #8852, #7290, #55, #6399, #1719, #4140, #3363, #3213, #7963, #836, #1045, #2534, #5579, #9576, #6498, #1811, #4190, #4763, #7340, #1665, #1762, #213, #7188, #894, #9677, #2480, #5634, #2585, #8800, #8742, #2384, #5730, #1614, #7138, #6349, #4864, #9527, #8010, #4087, #156, #8365, #9874, #1287, #9727, #9156, #7438, #2013, #5168, #7593 ),
 .UNSPECIFIED., .F., .T. ) 
 B_SPLINE_CURVE_WITH_KNOTS ( ( 3, 2, 2, 2, 2, 2, 2, 2, 2, 2, 2, 2, 2, 2, 2, 2, 2, 2, 2, 2, 2, 2, 2, 2, 2, 2, 2, 2, 2, 2, 2, 2, 2, 2, 2, 2, 2, 2, 2, 2, 2, 2, 2, 2, 2, 2, 2, 2, 2, 2, 2, 2, 2, 2, 2, 2, 2, 2, 2, 2, 2, 2, 2, 2, 2, 3 ),
 ( 0.000000000000000000, 0.01428571428571428527, 0.02857142857142857054, 0.04285714285714285060, 0.05714285714285714107, 0.07142857142857142461, 0.08571428571428570120, 0.1000000000000000056, 0.1142857142857142821, 0.1285714285714285587, 0.1428571428571428492, 0.1571428571428571397, 0.1714285714285714024, 0.1857142857142857206, 0.2000000000000000111, 0.2142857142857142738, 0.2285714285714285643, 0.2428571428571428548, 0.2571428571428571175, 0.2714285714285714080, 0.2857142857142856984, 0.2999999999999999889, 0.3142857142857142794, 0.3285714285714285698, 0.3428571428571428048, 0.3571428571428571508, 0.3714285714285714413, 0.3857142857142857317, 0.4000000000000000222, 0.4142857142857143127, 0.4285714285714285476, 0.4428571428571428381, 0.4571428571428571286, 0.4714285714285714191, 0.4857142857142857095, 0.5000000000000000000, 0.5142857142857142350, 0.5285714285714285809, 0.5428571428571428159, 0.5571428571428571619, 0.5714285714285713969, 0.5857142857142857428, 0.5999999999999999778, 0.6142857142857143238, 0.6285714285714285587, 0.6428571428571429047, 0.6571428571428571397, 0.6714285714285713746, 0.6857142857142856096, 0.6999999999999999556, 0.7142857142857143016, 0.7285714285714285365, 0.7428571428571428825, 0.7571428571428571175, 0.7714285714285714635, 0.7857142857142856984, 0.8000000000000000444, 0.8142857142857143904, 0.8285714285714286254, 0.8428571428571428603, 0.8571428571428570953, 0.8714285714285714413, 0.8857142857142856762, 0.9000000000000000222, 0.9142857142857142572, 0.9285714285714286031 ),
 .UNSPECIFIED. ) 
 CURVE ( )  GEOMETRIC_REPRESENTATION_ITEM ( )  RATIONAL_B_SPLINE_CURVE ( ( 1.000000000000000000, 0.9510565162951535312, 1.000000000000000000, 0.9510565162951535312, 1.000000000000000000, 0.9510565162951535312, 1.000000000000000000, 0.9510565162951535312, 1.000000000000000000, 0.9510565162951535312, 1.000000000000000000, 0.9510565162951535312, 1.000000000000000000, 0.9510565162951535312, 1.000000000000000000, 0.9510565162951535312, 1.000000000000000000, 0.9510565162951535312, 1.000000000000000000, 0.9510565162951535312, 1.000000000000000000, 0.9510565162951535312, 1.000000000000000000, 0.9510565162951535312, 1.000000000000000000, 0.9510565162951535312, 1.000000000000000000, 0.9510565162951535312, 1.000000000000000000, 0.9510565162951535312, 1.000000000000000000, 0.9510565162951535312, 1.000000000000000000, 0.9510565162951535312, 1.000000000000000000, 0.9510565162951535312, 1.000000000000000000, 0.9510565162951535312, 1.000000000000000000, 0.9510565162951535312, 1.000000000000000000, 0.9510565162951535312, 1.000000000000000000, 0.9510565162951535312, 1.000000000000000000, 0.9510565162951535312, 1.000000000000000000, 0.9510565162951535312, 1.000000000000000000, 0.9510565162951535312, 1.000000000000000000, 0.9510565162951535312, 1.000000000000000000, 0.9510565162951535312, 1.000000000000000000, 0.9510565162951535312, 1.000000000000000000, 0.9510565162951535312, 1.000000000000000000, 0.9510565162951535312, 1.000000000000000000, 0.9510565162951535312, 1.000000000000000000, 0.9510565162951535312, 1.000000000000000000, 0.9510565162951535312, 1.000000000000000000, 0.9510565162951535312, 1.000000000000000000, 0.9510565162951535312, 1.000000000000000000, 0.9510565162951535312, 1.000000000000000000, 0.9510565162951535312, 1.000000000000000000, 0.9510565162951535312, 1.000000000000000000, 0.9510565162951535312, 1.000000000000000000, 0.9510565162951535312, 1.000000000000000000, 0.9510565162951535312, 1.000000000000000000, 0.9510565162951535312, 1.000000000000000000, 0.9510565162951535312, 1.000000000000000000, 0.9510565162951535312, 1.000000000000000000, 0.9510565162951535312, 1.000000000000000000, 0.9510565162951535312, 1.000000000000000000, 0.9510565162951535312, 1.000000000000000000, 0.9510565162951535312, 1.000000000000000000, 0.9510565162951535312, 1.000000000000000000, 0.9510565162951535312, 1.000000000000000000, 0.9510565162951535312, 1.000000000000000000, 0.9510565162951535312, 1.000000000000000000, 0.9510565162951535312, 1.000000000000000000, 0.9510565162951535312, 1.000000000000000000, 0.9510565162951535312, 1.000000000000000000, 0.9510565162951535312, 1.000000000000000000, 0.9510565162951535312, 1.000000000000000000, 0.9510565162951535312, 1.000000000000000000, 0.9510565162951535312, 1.000000000000000000, 0.9510565162951535312, 1.000000000000000000, 0.9510565162951535312, 1.000000000000000000, 0.9510565162951535312, 1.000000000000000000, 0.9510565162951535312, 1.000000000000000000, 0.9510565162951535312, 1.000000000000000000, 0.9510565162951535312, 1.000000000000000000 ) ) 
 REPRESENTATION_ITEM ( '' )  );
#331 = CYLINDRICAL_SURFACE ( 'NONE', #1163, 15.44569104238500046 ) ;
#332 = CARTESIAN_POINT ( 'NONE',  ( 13.82664651025767100, -8.841785722321541030, 36.78975485534072476 ) ) ;
#333 = CARTESIAN_POINT ( 'NONE',  ( 7.448449071214646722, 11.85413878919601594, 37.28571428571429180 ) ) ;
#334 = CARTESIAN_POINT ( 'NONE',  ( -9.899494936611716867, 9.899494936611610285, 42.00000000000000000 ) ) ;
#335 = EDGE_LOOP ( 'NONE', ( #1912, #1497, #4062, #8563 ) ) ;
#336 = AXIS2_PLACEMENT_3D ( 'NONE', #4011, #10212, #2306 ) ;
#337 = CARTESIAN_POINT ( 'NONE',  ( -11.60466159355861926, -11.60466159355875249, 40.50000000000000711 ) ) ;
#338 = CARTESIAN_POINT ( 'NONE',  ( -5.853818627049699685, 14.80933238498958282, -1.389475189636273717E-15 ) ) ;
#339 = AXIS2_PLACEMENT_3D ( 'NONE', #8130, #857, #5651 ) ;
#340 = CARTESIAN_POINT ( 'NONE',  ( -15.89939535829186923, -1.791431617653016062, 23.14285714285714590 ) ) ;
#341 = DIRECTION ( 'NONE',  ( -0.9575619921529162637, -0.2882273949230683141, -3.311798021194104978E-34 ) ) ;
#342 = CARTESIAN_POINT ( 'NONE',  ( -4.270415729527831772, -8.486213763410670907, 15.09886208192144430 ) ) ;
#343 = CARTESIAN_POINT ( 'NONE',  ( 9.390499931835536884, -1.439022436064273158, 8.198862081921454603 ) ) ;
#344 = CARTESIAN_POINT ( 'NONE',  ( -11.69682198916834892, -11.51250119794901394, 8.504040569626438284 ) ) ;
#345 = VECTOR ( 'NONE', #3233, 1000.000000000000000 ) ;
#346 = CARTESIAN_POINT ( 'NONE',  ( 15.49051278174638036, 5.420364854932175014, 25.92857142857142705 ) ) ;
#347 = PRESENTATION_LAYER_ASSIGNMENT (  '', '', ( #4963 ) ) ;
#348 = VECTOR ( 'NONE', #8424, 1000.000000000000000 ) ;
#349 =( NAMED_UNIT ( * ) SI_UNIT ( $, .STERADIAN. ) SOLID_ANGLE_UNIT ( ) );
#350 = CARTESIAN_POINT ( 'NONE',  ( -1.707986654103994528, 16.32287076676380266, 10.64689771248357886 ) ) ;
#351 = CARTESIAN_POINT ( 'NONE',  ( 13.91197093850538380, 1.567502665446386390, 26.14285714285714590 ) ) ;
#352 = CARTESIAN_POINT ( 'NONE',  ( 16.30827793483735633, -1.837501619626142890, 8.357142857142855874 ) ) ;
#353 = CARTESIAN_POINT ( 'NONE',  ( -4.724406229267374968, -9.377220287599040915, 9.098862081921437195 ) ) ;
#354 = ORIENTED_EDGE ( 'NONE', *, *, #6522, .T. ) ;
#355 = CARTESIAN_POINT ( 'NONE',  ( -13.91197093850538380, -1.567502665446387278, 17.14285714285713880 ) ) ;
#356 = ORIENTED_EDGE ( 'NONE', *, *, #8845, .T. ) ;
#357 =( GEOMETRIC_REPRESENTATION_CONTEXT ( 3 ) GLOBAL_UNCERTAINTY_ASSIGNED_CONTEXT ( ( #1022 ) ) GLOBAL_UNIT_ASSIGNED_CONTEXT ( ( #599, #1315, #9183 ) ) REPRESENTATION_CONTEXT ( 'NONE', 'WORKASPACE' ) );
#358 =( GEOMETRIC_REPRESENTATION_CONTEXT ( 3 ) GLOBAL_UNCERTAINTY_ASSIGNED_CONTEXT ( ( #7416 ) ) GLOBAL_UNIT_ASSIGNED_CONTEXT ( ( #3591, #997, #9684 ) ) REPRESENTATION_CONTEXT ( 'NONE', 'WORKASPACE' ) );
#359 = CARTESIAN_POINT ( 'NONE',  ( 11.31370849898482334, -11.31370849898469366, 27.00000000000000355 ) ) ;
#360 = CARTESIAN_POINT ( 'NONE',  ( 1.665163862719847732, 15.91362231745477374, 50.85310228751642825 ) ) ;
#361 = CARTESIAN_POINT ( 'NONE',  ( 7.424621202458790314, -7.424621202458697944, 16.50000000000001421 ) ) ;
#362 = CARTESIAN_POINT ( 'NONE',  ( -13.55419868402807992, -4.742819248065651472, 10.92857142857143060 ) ) ;
#363 = CARTESIAN_POINT ( 'NONE',  ( 11.78653521626494793, 7.556039541191463371, 33.71024514465927524 ) ) ;
#364 = ORIENTED_EDGE ( 'NONE', *, *, #6954, .T. ) ;
#365 =( LENGTH_UNIT ( ) NAMED_UNIT ( * ) SI_UNIT ( .MILLI., .METRE. ) );
#366 = LINE ( 'NONE', #6691, #7331 ) ;
#367 = CARTESIAN_POINT ( 'NONE',  ( -7.027753727702738651, -7.098671581784268270, 3.248862081921429112 ) ) ;
#368 = CARTESIAN_POINT ( 'NONE',  ( -1.737328882695368115, 14.25515036105620581, 50.63881657323071295 ) ) ;
#369 = AXIS2_PLACEMENT_3D ( 'NONE', #442, #2961, #1373 ) ;
#370 = CARTESIAN_POINT ( 'NONE',  ( 7.390897758835871301, -7.458344646081617846, 15.50113791807859620 ) ) ;
#371 = CARTESIAN_POINT ( 'NONE',  ( -1.776620879821455556, -10.89658364409025637, 0.9511379180785689558 ) ) ;
#372 = DIRECTION ( 'NONE',  ( -1.000000000000000000, 0.000000000000000000, -0.000000000000000000 ) ) ;
#373 = CARTESIAN_POINT ( 'NONE',  ( -12.08964793087886314, 7.750357176954159932, 21.78975485534072476 ) ) ;
#374 = SURFACE_SIDE_STYLE ('',( #9112 ) ) ;
#375 = CARTESIAN_POINT ( 'NONE',  ( 10.24623928997352884, 10.06191849875416899, 23.50404056962643295 ) ) ;
#376 = CARTESIAN_POINT ( 'NONE',  ( 9.837026868206066865, -5.012215536711392083, 7.350000000000000533 ) ) ;
#377 = CARTESIAN_POINT ( 'NONE',  ( 8.404922754268618235, 13.61519076058357491, 45.28167371608785174 ) ) ;
#378 = EDGE_LOOP ( 'NONE', ( #1327, #9826 ) ) ;
#379 = CARTESIAN_POINT ( 'NONE',  ( -11.25295468363732709, 9.057666965552700233, 48.73000000000003951 ) ) ;
#380 = DIRECTION ( 'NONE',  ( 0.000000000000000000, 1.000000000000000000, 0.000000000000000000 ) ) ;
#381 = CARTESIAN_POINT ( 'NONE',  ( -9.375578539472099848, 1.533232399700011461, 4.701137918078535982 ) ) ;
#382 = CARTESIAN_POINT ( 'NONE',  ( -6.717514421272238856, 6.717514421272181124, 12.00000000000001066 ) ) ;
#383 = AXIS2_PLACEMENT_3D ( 'NONE', #7978, #9740, #5647 ) ;
#384 = CARTESIAN_POINT ( 'NONE',  ( 0.2000000000000057288, 2.703062956522977593E-33, 3.299999999999999822 ) ) ;
#385 = CARTESIAN_POINT ( 'NONE',  ( 4.742819248065503146, 13.55419868402813677, 25.07142857142858361 ) ) ;
#386 = VECTOR ( 'NONE', #1036, 1000.000000000000000 ) ;
#387 = CARTESIAN_POINT ( 'NONE',  ( 4.742819248065503146, 13.55419868402813677, 43.07142857142858361 ) ) ;
#388 = ORIENTED_EDGE ( 'NONE', *, *, #1909, .T. ) ;
#389 = CARTESIAN_POINT ( 'NONE',  ( -5.284464991282755264, 15.10213328493384743, 42.42857142857143060 ) ) ;
#390 = FACE_OUTER_BOUND ( 'NONE', #54, .T. ) ;
#391 = CARTESIAN_POINT ( 'NONE',  ( -11.60466159355861926, -11.60466159355875249, 10.50000000000000533 ) ) ;
#392 = FILL_AREA_STYLE ('',( #2563 ) ) ;
#393 = PRODUCT_DEFINITION_SHAPE ( 'NONE', 'NONE',  #8011 ) ;
#394 = ADVANCED_FACE ( 'NONE', ( #8448 ), #10092, .T. ) ;
#395 = CARTESIAN_POINT ( 'NONE',  ( 56.99999999999997158, 0.000000000000000000, 0.000000000000000000 ) ) ;
#396 = CARTESIAN_POINT ( 'NONE',  ( 8.442910196168311288, 4.355403765523576887, 16.89886208192141126 ) ) ;
#397 = CARTESIAN_POINT ( 'NONE',  ( -8.922933199037192509, 4.490180821391428267, 3.848862081921410105 ) ) ;
#398 = UNCERTAINTY_MEASURE_WITH_UNIT (LENGTH_MEASURE( 1.000000000000000082E-05 ), #6272, 'distance_accuracy_value', 'NONE');
#399 = CARTESIAN_POINT ( 'NONE',  ( 1.917699372585825790, 15.88516839912900203, 4.861183426769296823 ) ) ;
#400 = CARTESIAN_POINT ( 'NONE',  ( -8.731428362939189114, 13.89598863503036341, 36.21428571428573662 ) ) ;
#401 = ADVANCED_FACE ( 'NONE', ( #10107 ), #1214, .F. ) ;
#402 = VECTOR ( 'NONE', #5225, 1000.000000000000000 ) ;
#403 = CARTESIAN_POINT ( 'NONE',  ( 5.543385399275644332, 15.44746603149420494, 11.07546914105500768 ) ) ;
#404 = CARTESIAN_POINT ( 'NONE',  ( 7.448449071214646722, 11.85413878919601594, 19.28571428571428825 ) ) ;
#405 = LINE ( 'NONE', #3548, #2162 ) ;
#406 = CARTESIAN_POINT ( 'NONE',  ( -13.89598863503046111, 8.731428362939027465, 47.78571428571430602 ) ) ;
#407 = ORIENTED_EDGE ( 'NONE', *, *, #4270, .T. ) ;
#408 = CARTESIAN_POINT ( 'NONE',  ( -12.15899005565164792, 7.639999817571651697, 17.78571428571428115 ) ) ;
#409 = CARTESIAN_POINT ( 'NONE',  ( -11.60466159355861748, -11.60466159355874893, 28.50000000000000000 ) ) ;
#410 = CARTESIAN_POINT ( 'NONE',  ( -16.32287076676382398, 1.707986654103809343, 49.35310228751642114 ) ) ;
#411 = CARTESIAN_POINT ( 'NONE',  ( -10.37072757624895836, 1.642561882922380923, 17.69999999999999218 ) ) ;
#412 = CARTESIAN_POINT ( 'NONE',  ( 4.742819248065502258, 13.55419868402813499, 7.071428571428569398 ) ) ;
#413 = EDGE_LOOP ( 'NONE', ( #2584, #9697, #9041, #6358 ) ) ;
#414 = CARTESIAN_POINT ( 'NONE',  ( 13.89774397934249706, 1.693770420379375308, 28.13881657323070939 ) ) ;
#415 =( NAMED_UNIT ( * ) SI_UNIT ( $, .STERADIAN. ) SOLID_ANGLE_UNIT ( ) );
#416 = CARTESIAN_POINT ( 'NONE',  ( -166.6500000000000341, -1.532656777835077474E-15, 13.00000000000000355 ) ) ;
#417 = EDGE_CURVE ( 'NONE', #5816, #3063, #2247, .T. ) ;
#418 = CARTESIAN_POINT ( 'NONE',  ( 6.751237864895159646, -6.683790977649233689, 5.498862081921462419 ) ) ;
#419 = CARTESIAN_POINT ( 'NONE',  ( 7.340858601237956194, 11.92174236212700045, 51.28167371608785174 ) ) ;
#420 = CARTESIAN_POINT ( 'NONE',  ( -10.90442828429183919, -1.727091770866655329, 5.549999999999999822 ) ) ;
#421 = CARTESIAN_POINT ( 'NONE',  ( -10.91227292449344155, -1.677562661911748965, 4.551137918078585365 ) ) ;
#422 = DIRECTION ( 'NONE',  ( -1.000000000000000000, -0.000000000000000000, -0.000000000000000000 ) ) ;
#423 = CARTESIAN_POINT ( 'NONE',  ( 4.865839792409144771, 13.51115193377589740, 29.07546914105501301 ) ) ;
#424 = CARTESIAN_POINT ( 'NONE',  ( 4.766900247265192903, 9.355568503977911732, 9.599999999999997868 ) ) ;
#425 = CARTESIAN_POINT ( 'NONE',  ( -16.32287076676382398, 1.707986654103809343, 43.35310228751642825 ) ) ;
#426 = CARTESIAN_POINT ( 'NONE',  ( -5.462592421889175043, 15.04626098580285998, 48.73000000000003951 ) ) ;
#427 = CARTESIAN_POINT ( 'NONE',  ( 5.420364854932001819, 15.49051278174644430, 25.07142857142858361 ) ) ;
#428 = CARTESIAN_POINT ( 'NONE',  ( 15.44569104238500046, -1.018491042385001544, -1.270000000000007123 ) ) ;
#429 = EDGE_CURVE ( 'NONE', #7540, #5816, #4809, .T. ) ;
#430 = CARTESIAN_POINT ( 'NONE',  ( -9.989344678689363377, 9.809645194533960222, 13.99595943037356527 ) ) ;
#431 = CARTESIAN_POINT ( 'NONE',  ( -6.683790977649319842, 6.751237864895094809, 14.00113791807859620 ) ) ;
#432 = CARTESIAN_POINT ( 'NONE',  ( 9.873755945037075321, 1.513077731353043909, 0.05113791807855379290 ) ) ;
#433 = EDGE_CURVE ( 'NONE', #9051, #3839, #8410, .T. ) ;
#434 = CARTESIAN_POINT ( 'NONE',  ( -162.8500000000000512, -5.808233104102145682E-15, 0.000000000000000000 ) ) ;
#435 = CARTESIAN_POINT ( 'NONE',  ( 16.29368510291089223, -1.967016585148476882, 36.36118342676930126 ) ) ;
#436 = CARTESIAN_POINT ( 'NONE',  ( -9.899494936611716867, 9.899494936611610285, 24.00000000000000000 ) ) ;
#437 = CARTESIAN_POINT ( 'NONE',  ( -4.623906867372410190, 13.21436662431711895, 42.42857142857143060 ) ) ;
#438 = EDGE_LOOP ( 'NONE', ( #4414, #892, #4751, #3837 ) ) ;
#439 = CARTESIAN_POINT ( 'NONE',  ( -13.89598863503046111, 8.731428362939027465, 47.78571428571430602 ) ) ;
#440 = DIRECTION ( 'NONE',  ( -1.000000000000000000, -0.000000000000000000, -0.000000000000000000 ) ) ;
#441 = CARTESIAN_POINT ( 'NONE',  ( -8.731428362939189114, 13.89598863503036341, 36.21428571428573662 ) ) ;
#442 = CARTESIAN_POINT ( 'NONE',  ( 0.000000000000000000, 18.00000000000000000, 0.000000000000000000 ) ) ;
#443 = FILL_AREA_STYLE ('',( #9851 ) ) ;
#444 = CARTESIAN_POINT ( 'NONE',  ( 1.513077731352925115, 9.873755945037103743, 16.44886208192140131 ) ) ;
#445 = CARTESIAN_POINT ( 'NONE',  ( 9.858066664633883036, 1.612135949262857082, 11.04886208192144359 ) ) ;
#446 = CARTESIAN_POINT ( 'NONE',  ( -5.012215536711506658, 9.837026868206027785, 15.14999999999998259 ) ) ;
#447 = CARTESIAN_POINT ( 'NONE',  ( -5.164528828830334817, 15.14410076328347543, 4.432611998197859116 ) ) ;
#448 = CARTESIAN_POINT ( 'NONE',  ( 8.512513224245308763, 13.54758718765259040, 25.28571428571428470 ) ) ;
#449 = AXIS2_PLACEMENT_3D ( 'NONE', #4004, #8752, #7976 ) ;
#450 = CARTESIAN_POINT ( 'NONE',  ( -15.53355953199861794, -5.297344310588530725, 2.932611998197868886 ) ) ;
#451 = APPLICATION_CONTEXT ( 'automotive_design' ) ;
#452 = CARTESIAN_POINT ( 'NONE',  ( 14.26974319298268767, -1.607813917172876916, 26.35714285714285765 ) ) ;
#453 = CARTESIAN_POINT ( 'NONE',  ( 1.791431617652837316, 15.89939535829188877, 6.857142857142860315 ) ) ;
#454 = CARTESIAN_POINT ( 'NONE',  ( 1.837501619626330074, -16.30827793483733501, 39.64285714285716722 ) ) ;
#455 = ORIENTED_EDGE ( 'NONE', *, *, #7282, .T. ) ;
#456 = CARTESIAN_POINT ( 'NONE',  ( 9.899494936611718643, -9.899494936611608509, 15.00000000000000000 ) ) ;
#457 = EDGE_CURVE ( 'NONE', #4209, #166, #5446, .T. ) ;
#458 = ORIENTED_EDGE ( 'NONE', *, *, #1070, .T. ) ;
#459 = AXIS2_PLACEMENT_3D ( 'NONE', #4903, #3979, #7954 ) ;
#460 = CARTESIAN_POINT ( 'NONE',  ( 15.89939535829187278, 1.791431617653015174, 38.14285714285714590 ) ) ;
#461 = CARTESIAN_POINT ( 'NONE',  ( 8.404922754268618235, 13.61519076058357491, 45.28167371608785174 ) ) ;
#462 = CARTESIAN_POINT ( 'NONE',  ( -5.056896391392315948, 9.814260835640997271, 1.148862081921408151 ) ) ;
#463 = SHAPE_DEFINITION_REPRESENTATION ( #3602, #1843 ) ;
#464 = CARTESIAN_POINT ( 'NONE',  ( 13.55419868402807992, 4.742819248065649695, 7.928571428571430602 ) ) ;
#465 = ORIENTED_EDGE ( 'NONE', *, *, #2286, .F. ) ;
#466 = CARTESIAN_POINT ( 'NONE',  ( 4.743843029824831525, -13.17239914596749095, 23.42453085894499409 ) ) ;
#467 = EDGE_LOOP ( 'NONE', ( #5213, #7257 ) ) ;
#468 = DIRECTION ( 'NONE',  ( 1.000000000000000000, 4.755747939841215952E-17, -0.000000000000000000 ) ) ;
#469 = CARTESIAN_POINT ( 'NONE',  ( -8.442910196168309511, -4.355403765523544024, 3.398862081921444123 ) ) ;
#470 = CARTESIAN_POINT ( 'NONE',  ( -4.766900247265192014, -9.355568503977867323, 8.099999999999996092 ) ) ;
#471 = CARTESIAN_POINT ( 'NONE',  ( -10.91227292449344155, -1.677562661911748965, 7.551137918078578259 ) ) ;
#472 = DIRECTION ( 'NONE',  ( -1.000000000000000000, -1.387778780781445676E-16, -0.000000000000000000 ) ) ;
#473 = CARTESIAN_POINT ( 'NONE',  ( -1.642561882922479732, 10.37072757624895303, 3.299999999999969624 ) ) ;
#474 = CARTESIAN_POINT ( 'NONE',  ( 13.96533075980324234, -8.621071003556521006, 40.78167371608785885 ) ) ;
#475 = CARTESIAN_POINT ( 'NONE',  ( -10.53772368660228231, 9.764597359209851390, 48.73000000000002530 ) ) ;
#476 = CARTESIAN_POINT ( 'NONE',  ( 11.31370849898482334, -11.31370849898469366, 21.00000000000000355 ) ) ;
#477 = CARTESIAN_POINT ( 'NONE',  ( 2.000000000000001776, -0.8865213383406622683, -1.535500000000078469 ) ) ;
#478 = CARTESIAN_POINT ( 'NONE',  ( -9.989344678689363377, 9.809645194533960222, 19.99595943037356349 ) ) ;
#479 = CARTESIAN_POINT ( 'NONE',  ( -9.375578539472099848, 1.533232399700011461, 13.70113791807854398 ) ) ;
#480 = CARTESIAN_POINT ( 'NONE',  ( 7.063212654743467489, 7.063212654743559860, 18.74999999999998934 ) ) ;
#481 = DIRECTION ( 'NONE',  ( 0.000000000000000000, -1.000000000000000000, 0.000000000000000000 ) ) ;
#482 = CARTESIAN_POINT ( 'NONE',  ( 15.53355953199861794, 5.297344310588528060, 41.93261199819787066 ) ) ;
#483 = CARTESIAN_POINT ( 'NONE',  ( 12.15899005565164792, -7.639999817571655250, 44.78571428571428470 ) ) ;
#484 = CARTESIAN_POINT ( 'NONE',  ( -7.448449071214644945, -11.85413878919601771, 34.28571428571428470 ) ) ;
#485 = ORIENTED_EDGE ( 'NONE', *, *, #7973, .F. ) ;
#486 = CARTESIAN_POINT ( 'NONE',  ( -8.841785722321695573, 13.82664651025757152, 2.210245144659280569 ) ) ;
#487 = DIRECTION ( 'NONE',  ( 0.000000000000000000, -6.338944243255235518E-49, 1.000000000000000000 ) ) ;
#488 = CARTESIAN_POINT ( 'NONE',  ( -15.49051278174638036, -5.420364854932175902, 28.92857142857143771 ) ) ;
#489 = DIRECTION ( 'NONE',  ( 1.000000000000000000, 0.000000000000000000, 0.000000000000000000 ) ) ;
#490 = CARTESIAN_POINT ( 'NONE',  ( -55.00000000000002132, 7.703719777548943412E-30, -7.703719777548943412E-31 ) ) ;
#491 = CARTESIAN_POINT ( 'NONE',  ( -7.806708723663830618, -7.806708723663906113, 2.249999999999986233 ) ) ;
#492 = CARTESIAN_POINT ( 'NONE',  ( -9.865911304835474738, -1.562606840307925626, 5.549999999999999822 ) ) ;
#493 = CARTESIAN_POINT ( 'NONE',  ( 9.858066664633883036, 1.612135949262857082, 8.048862081921450695 ) ) ;
#494 = PRODUCT_DEFINITION_CONTEXT ( 'detailed design', #8367, 'design' ) ;
#495 = CARTESIAN_POINT ( 'NONE',  ( -4.766900247265192014, -9.355568503977876205, 17.10000000000000497 ) ) ;
#496 = CARTESIAN_POINT ( 'NONE',  ( -16.29368510291090288, 1.967016585148476215, 15.36118342676929771 ) ) ;
#497 = CARTESIAN_POINT ( 'NONE',  ( 15.89939535829187278, 1.791431617653015174, 38.14285714285714590 ) ) ;
#498 = CARTESIAN_POINT ( 'NONE',  ( -15.53355953199861794, -5.297344310588530725, 8.932611998197868886 ) ) ;
#499 = AXIS2_PLACEMENT_3D ( 'NONE', #9498, #7831, #2505 ) ;
#500 = CARTESIAN_POINT ( 'NONE',  ( -13.91197093850538380, -1.567502665446387278, 23.14285714285714590 ) ) ;
#501 = CARTESIAN_POINT ( 'NONE',  ( 1.837501619626330074, -16.30827793483733501, 9.642857142857147679 ) ) ;
#502 = CARTESIAN_POINT ( 'NONE',  ( 1.791431617652837316, 15.89939535829188877, 48.85714285714286120 ) ) ;
#503 = VERTEX_POINT ( 'NONE', #9443 ) ;
#504 = CARTESIAN_POINT ( 'NONE',  ( 7.424621202458790314, -7.424621202458697944, 16.50000000000001421 ) ) ;
#505 = ORIENTED_EDGE ( 'NONE', *, *, #1535, .T. ) ;
#506 = CARTESIAN_POINT ( 'NONE',  ( 5.420364854932000931, 15.49051278174644075, 31.07142857142857295 ) ) ;
#507 = MECHANICAL_DESIGN_GEOMETRIC_PRESENTATION_REPRESENTATION (  '', ( #4963 ), #2980 ) ;
#508 = AXIS2_PLACEMENT_3D ( 'NONE', #384, #7615, #536 ) ;
#509 = CARTESIAN_POINT ( 'NONE',  ( -1.967016585148659846, 16.29368510291087091, 50.63881657323071295 ) ) ;
#510 = CARTESIAN_POINT ( 'NONE',  ( -10.90442828429183919, -1.727091770866654663, 14.55000000000000249 ) ) ;
#511 = CARTESIAN_POINT ( 'NONE',  ( -15.10213328493390961, 5.284464991282586510, 5.571428571428574728 ) ) ;
#512 = PRODUCT_CONTEXT ( 'NONE', #7716, 'mechanical' ) ;
#513 = CARTESIAN_POINT ( 'NONE',  ( 11.85413878919593422, 7.448449071214774619, 31.71428571428571530 ) ) ;
#514 = CIRCLE ( 'NONE', #1996, 0.2000000000000000944 ) ;
#515 = ORIENTED_EDGE ( 'NONE', *, *, #5831, .F. ) ;
#516 = CARTESIAN_POINT ( 'NONE',  ( 9.989344678689365153, -9.809645194533958446, 34.99595943037355994 ) ) ;
#517 = ORIENTED_EDGE ( 'NONE', *, *, #4719, .F. ) ;
#518 = DIRECTION ( 'NONE',  ( 0.7063021515967569108, 0.7063021515967620179, -0.04769215134145658730 ) ) ;
#519 = CARTESIAN_POINT ( 'NONE',  ( -13.96533075980324234, 8.621071003556515677, 7.781673716087849968 ) ) ;
#520 = CARTESIAN_POINT ( 'NONE',  ( -108.0000000000000426, 18.00000000000000355, 0.000000000000000000 ) ) ;
#521 = CARTESIAN_POINT ( 'NONE',  ( 9.858066664633883036, 1.612135949262857526, 5.048862081921459577 ) ) ;
#522 = CARTESIAN_POINT ( 'NONE',  ( 11.78653521626494793, 7.556039541191463371, 45.71024514465928235 ) ) ;
#523 = CARTESIAN_POINT ( 'NONE',  ( 1.727091770866550968, 10.90442828429186761, 6.449999999999969091 ) ) ;
#524 = CARTESIAN_POINT ( 'NONE',  ( -10.36326688006724162, 1.689666864740236640, 13.70113791807854398 ) ) ;
#525 = DIRECTION ( 'NONE',  ( 0.000000000000000000, 1.000000000000000000, -1.332267629550187849E-15 ) ) ;
#526 = CARTESIAN_POINT ( 'NONE',  ( -4.865839792409144771, -13.51115193377589740, 26.07546914105500235 ) ) ;
#527 = CARTESIAN_POINT ( 'NONE',  ( -7.806708723663830618, -7.806708723663902560, 14.25000000000001243 ) ) ;
#528 = CARTESIAN_POINT ( 'NONE',  ( 16.32287076676382043, -1.707986654103810897, 40.35310228751642825 ) ) ;
#529 = CIRCLE ( 'NONE', #2831, 17.72919999999999874 ) ;
#530 = CARTESIAN_POINT ( 'NONE',  ( -8.057929360137700669, 13.68023991280794149, 48.73000000000005372 ) ) ;
#531 = AXIS2_PLACEMENT_3D ( 'NONE', #7567, #3693, #489 ) ;
#532 = CARTESIAN_POINT ( 'NONE',  ( 4.995402070941135086, -13.58603705635637304, -1.270000000000007123 ) ) ;
#533 = CARTESIAN_POINT ( 'NONE',  ( 4.619798703721856192, 13.59724543428036725, 21.06738800180213644 ) ) ;
#534 = CARTESIAN_POINT ( 'NONE',  ( -4.355403765523468529, -8.442910196168352144, 13.10113791807856920 ) ) ;
#535 = CARTESIAN_POINT ( 'NONE',  ( -9.375578539472099848, 1.533232399700010351, 7.701137918078540423 ) ) ;
#536 = DIRECTION ( 'NONE',  ( 0.000000000000000000, -8.191099868251441548E-34, -1.000000000000000000 ) ) ;
#537 = CARTESIAN_POINT ( 'NONE',  ( -1.707986654103994528, 16.32287076676380266, 40.64689771248358596 ) ) ;
#538 = CARTESIAN_POINT ( 'NONE',  ( -14.26974319298268767, 1.607813917172874918, 41.35714285714286120 ) ) ;
#539 = CARTESIAN_POINT ( 'NONE',  ( -13.17239914596754424, 4.743843029824683200, 3.575469141055005462 ) ) ;
#540 = ORIENTED_EDGE ( 'NONE', *, *, #3932, .F. ) ;
#541 = CARTESIAN_POINT ( 'NONE',  ( -8.512513224245306986, -13.54758718765259218, 40.28571428571428470 ) ) ;
#542 = CARTESIAN_POINT ( 'NONE',  ( -11.31370849898482156, 11.31370849898469544, 0.000000000000000000 ) ) ;
#543 = CARTESIAN_POINT ( 'NONE',  ( 13.54758718765249803, 8.512513224245457977, 25.71428571428571885 ) ) ;
#544 = CARTESIAN_POINT ( 'NONE',  ( -2.000000000000000888, -18.00000000000000355, 2.204364238465235822E-15 ) ) ;
#545 = CIRCLE ( 'NONE', #4999, 13.00000000000000533 ) ;
#546 = CARTESIAN_POINT ( 'NONE',  ( 1.727091770866550968, 10.90442828429187294, 0.4499999999999856337 ) ) ;
#547 = CARTESIAN_POINT ( 'NONE',  ( 6.717514421272239744, -6.717514421272154479, 4.500000000000003553 ) ) ;
#548 = CARTESIAN_POINT ( 'NONE',  ( 8.442910196168311288, 4.355403765523574222, 13.89886208192141126 ) ) ;
#549 = EDGE_CURVE ( 'NONE', #4723, #3726, #2398, .T. ) ;
#550 = CARTESIAN_POINT ( 'NONE',  ( 7.806708723663831506, 7.806708723663930982, 12.75000000000000533 ) ) ;
#551 = CARTESIAN_POINT ( 'NONE',  ( 5.543385399275644332, 15.44746603149420494, 17.07546914105500591 ) ) ;
#552 = CARTESIAN_POINT ( 'NONE',  ( 11.31370849898482334, -11.31370849898469366, 45.00000000000000711 ) ) ;
#553 = CARTESIAN_POINT ( 'NONE',  ( -8.620103694221995738, -13.47998361472161299, 26.28975485534072831 ) ) ;
#554 = CARTESIAN_POINT ( 'NONE',  ( 4.742819248065503146, 13.55419868402813677, 19.07142857142856940 ) ) ;
#555 = CARTESIAN_POINT ( 'NONE',  ( -13.89598863503046111, 8.731428362939027465, 5.785714285714282035 ) ) ;
#556 = CARTESIAN_POINT ( 'NONE',  ( -13.89598863503046111, 8.731428362939027465, 41.78571428571430602 ) ) ;
#557 = VERTEX_POINT ( 'NONE', #5547 ) ;
#558 = CARTESIAN_POINT ( 'NONE',  ( 9.355568503977840678, 4.766900247265305701, 18.90000000000002700 ) ) ;
#559 = ORIENTED_EDGE ( 'NONE', *, *, #2679, .F. ) ;
#560 = CARTESIAN_POINT ( 'NONE',  ( 1.837501619626329630, -16.30827793483733501, 39.64285714285715301 ) ) ;
#561 = ADVANCED_FACE ( 'NONE', ( #71, #5593 ), #1530, .F. ) ;
#562 = CARTESIAN_POINT ( 'NONE',  ( 15.44746603149413922, 5.543385399275817527, 45.92453085894500475 ) ) ;
#563 = CARTESIAN_POINT ( 'NONE',  ( -1.642561882922479732, 10.37072757624895303, 18.29999999999998295 ) ) ;
#564 = CARTESIAN_POINT ( 'NONE',  ( 15.10213328493390783, -5.284464991282587398, 2.571428571428571619 ) ) ;
#565 = CARTESIAN_POINT ( 'NONE',  ( 15.10213328493390783, -5.284464991282587398, 8.571428571428569398 ) ) ;
#566 = PRODUCT_RELATED_PRODUCT_CATEGORY ( 'part', '', ( #9805 ) ) ;
#567 = CARTESIAN_POINT ( 'NONE',  ( -13.91197093850538380, -1.567502665446387278, 23.14285714285714590 ) ) ;
#568 = ADVANCED_BREP_SHAPE_REPRESENTATION ( '', ( #3700, #3995 ), #9548 ) ;
#569 = CARTESIAN_POINT ( 'NONE',  ( 13.51115193377584589, 4.865839792409294873, 45.92453085894500475 ) ) ;
#570 = AXIS2_PLACEMENT_3D ( 'NONE', #1238, #4444, #4391 ) ;
#571 = EDGE_LOOP ( 'NONE', ( #1086, #3200, #2296, #1950 ) ) ;
#572 = DIRECTION ( 'NONE',  ( 0.000000000000000000, -6.338944243255235518E-49, 1.000000000000000000 ) ) ;
#573 = CARTESIAN_POINT ( 'NONE',  ( 1.665163862719847732, 15.91362231745477374, 20.85310228751641759 ) ) ;
#574 = LINE ( 'NONE', #8420, #9956 ) ;
#575 = CARTESIAN_POINT ( 'NONE',  ( -4.579542530753125895, 8.877401133907090625, 1.148862081921408151 ) ) ;
#576 = CARTESIAN_POINT ( 'NONE',  ( 1.441234910513245149, 13.92619789766829008, 50.85310228751642825 ) ) ;
#577 = CARTESIAN_POINT ( 'NONE',  ( 9.355568503977840678, 4.766900247265305701, 6.899999999999961275 ) ) ;
#578 = CARTESIAN_POINT ( 'NONE',  ( 1.776620879821457333, 10.89658364409028124, 17.45113791807857240 ) ) ;
#579 = CARTESIAN_POINT ( 'NONE',  ( 0.000000000000000000, 2.703062956522977593E-33, 3.299999999999999822 ) ) ;
#580 = SHAPE_REPRESENTATION_RELATIONSHIP ( 'NONE' , 'NONE' ,  #8907, #568 ) ;
#581 = CARTESIAN_POINT ( 'NONE',  ( 9.837026868206066865, -5.012215536711392083, 19.34999999999996945 ) ) ;
#582 = CARTESIAN_POINT ( 'NONE',  ( 5.404401153735178376, -15.06016580658422477, 47.42453085894499765 ) ) ;
#583 = CARTESIAN_POINT ( 'NONE',  ( 9.355568503977840678, 4.766900247265305701, 6.899999999999961275 ) ) ;
#584 = CARTESIAN_POINT ( 'NONE',  ( 5.284464991282756152, -15.10213328493384743, 27.42857142857143060 ) ) ;
#585 = EDGE_CURVE ( 'NONE', #5107, #8149, #1491, .T. ) ;
#586 = DIRECTION ( 'NONE',  ( 0.000000000000000000, -6.338944243255235518E-49, 1.000000000000000000 ) ) ;
#587 = CARTESIAN_POINT ( 'NONE',  ( -7.750357176954294935, 12.08964793087877787, 20.21024514465928235 ) ) ;
#588 = CARTESIAN_POINT ( 'NONE',  ( -6.683790977649319842, 6.751237864895094809, 11.00113791807855002 ) ) ;
#589 = CARTESIAN_POINT ( 'NONE',  ( -7.098671581784199880, -7.027753727702809705, 4.251137918078595312 ) ) ;
#590 = DIRECTION ( 'NONE',  ( -0.000000000000000000, 0.000000000000000000, -1.000000000000000000 ) ) ;
#591 = CARTESIAN_POINT ( 'NONE',  ( 13.82664651025767100, -8.841785722321541030, 42.78975485534072476 ) ) ;
#592 = CARTESIAN_POINT ( 'NONE',  ( -4.742819248065502258, -13.55419868402813677, 46.07142857142856940 ) ) ;
#593 = CARTESIAN_POINT ( 'NONE',  ( 13.21436662431716869, -4.623906867372263640, 44.57142857142857650 ) ) ;
#594 = VERTEX_POINT ( 'NONE', #10205 ) ;
#595 = CARTESIAN_POINT ( 'NONE',  ( -5.404401153735176599, 15.06016580658422477, 8.424530858944992318 ) ) ;
#596 = LINE ( 'NONE', #5391, #848 ) ;
#597 = CARTESIAN_POINT ( 'NONE',  ( -13.54758718765249625, -8.512513224245459753, 28.71428571428571530 ) ) ;
#598 = CARTESIAN_POINT ( 'NONE',  ( -4.995402070941133310, -13.58603705635637304, -1.270000000000007123 ) ) ;
#599 =( LENGTH_UNIT ( ) NAMED_UNIT ( * ) SI_UNIT ( .MILLI., .METRE. ) );
#600 = DIRECTION ( 'NONE',  ( -1.000000000000000000, -0.000000000000000000, -0.000000000000000000 ) ) ;
#601 = CARTESIAN_POINT ( 'NONE',  ( 1.486127417882244783, -9.383039235653782839, 10.80000000000003268 ) ) ;
#602 = CARTESIAN_POINT ( 'NONE',  ( 9.390499931835536884, -1.439022436064272936, 17.19886208192146171 ) ) ;
#603 = DIRECTION ( 'NONE',  ( -1.000000000000000000, 1.842239752758738928E-31, -1.780435181894459419E-32 ) ) ;
#604 = CARTESIAN_POINT ( 'NONE',  ( 8.731428362939190890, -13.89598863503036164, 45.21428571428572951 ) ) ;
#605 = FILL_AREA_STYLE ('',( #8456 ) ) ;
#606 = CARTESIAN_POINT ( 'NONE',  ( -11.22385875690717327, 11.40355824106234550, 16.00404056962643651 ) ) ;
#607 = ORIENTED_EDGE ( 'NONE', *, *, #8566, .T. ) ;
#608 = CARTESIAN_POINT ( 'NONE',  ( -1.607813917173034124, 14.26974319298267524, 30.64285714285715301 ) ) ;
#609 = ADVANCED_FACE ( 'NONE', ( #8706 ), #801, .F. ) ;
#610 = CARTESIAN_POINT ( 'NONE',  ( 11.60466159355862104, 11.60466159355875071, 13.50000000000000178 ) ) ;
#611 = CARTESIAN_POINT ( 'NONE',  ( -11.31370849898482156, 11.31370849898469544, 48.00000000000000000 ) ) ;
#612 = EDGE_LOOP ( 'NONE', ( #1014, #1623 ) ) ;
#613 = CARTESIAN_POINT ( 'NONE',  ( -7.424621202458789426, 7.424621202458724589, 18.00000000000001421 ) ) ;
#614 = SURFACE_STYLE_FILL_AREA ( #1388 ) ;
#615 = CARTESIAN_POINT ( 'NONE',  ( -5.284464991282755264, 15.10213328493384743, 48.42857142857143060 ) ) ;
#616 = ADVANCED_FACE ( 'NONE', ( #854 ), #3309, .F. ) ;
#617 = CARTESIAN_POINT ( 'NONE',  ( -7.771249796623103556, -7.842167650704634063, 6.248862081921465084 ) ) ;
#618 = CARTESIAN_POINT ( 'NONE',  ( 13.89598863503046111, -8.731428362939032795, 8.785714285714293581 ) ) ;
#619 = CARTESIAN_POINT ( 'NONE',  ( -5.284464991282755264, 15.10213328493384743, 0.4285714285714309346 ) ) ;
#620 =( LENGTH_UNIT ( ) NAMED_UNIT ( * ) SI_UNIT ( .MILLI., .METRE. ) );
#621 = CARTESIAN_POINT ( 'NONE',  ( 7.639999817571788476, -12.15899005565156266, 21.21428571428571530 ) ) ;
#622 = CARTESIAN_POINT ( 'NONE',  ( 1.478298951650704351, -14.28433602490913579, 25.64689771248357886 ) ) ;
#623 = AXIS2_PLACEMENT_3D ( 'NONE', #823, #981, #8843 ) ;
#624 = CARTESIAN_POINT ( 'NONE',  ( -7.750357176954294935, 12.08964793087877787, 44.21024514465928235 ) ) ;
#625 = ORIENTED_EDGE ( 'NONE', *, *, #2876, .T. ) ;
#626 = FACE_OUTER_BOUND ( 'NONE', #2874, .T. ) ;
#627 = CARTESIAN_POINT ( 'NONE',  ( 8.841785722321695573, -13.82664651025757152, 17.21024514465927879 ) ) ;
#628 = CARTESIAN_POINT ( 'NONE',  ( -8.731428362939187338, 13.89598863503036164, 0.2142857142857168273 ) ) ;
#629 = CARTESIAN_POINT ( 'NONE',  ( -1.533232399700100057, 9.375578539472098072, 7.298862081921430267 ) ) ;
#630 = CARTESIAN_POINT ( 'NONE',  ( -16.32287076676382398, 1.707986654103809343, 19.35310228751642825 ) ) ;
#631 = CARTESIAN_POINT ( 'NONE',  ( 10.90442828429183919, 1.727091770866678422, 4.049999999999988276 ) ) ;
#632 = CARTESIAN_POINT ( 'NONE',  ( -7.390897758835869524, 7.458344646081637386, 11.00113791807855002 ) ) ;
#633 = DIRECTION ( 'NONE',  ( 0.000000000000000000, -1.000000000000000000, 8.191099868251446680E-34 ) ) ;
#634 = CARTESIAN_POINT ( 'NONE',  ( 14.25515036105622535, -1.737328882695210241, 30.36118342676929771 ) ) ;
#635 = COLOUR_RGB ( '', 0.09019608, 0.27058824, 0.51372549) ;
#636 = CARTESIAN_POINT ( 'NONE',  ( -13.51115193377584589, -4.865839792409295761, 6.924530858944994982 ) ) ;
#637 = CARTESIAN_POINT ( 'NONE',  ( 1.727091770866551412, 10.90442828429187117, 3.450000000000007283 ) ) ;
#638 = CARTESIAN_POINT ( 'NONE',  ( -15.10213328493390961, 5.284464991282586510, 29.57142857142857650 ) ) ;
#639 = DIRECTION ( 'NONE',  ( 4.755747939841215952E-17, -1.000000000000000000, 0.000000000000000000 ) ) ;
#640 = AXIS2_PLACEMENT_3D ( 'NONE', #8513, #4066, #1542 ) ;
#641 = CARTESIAN_POINT ( 'NONE',  ( 7.750357176954296712, -12.08964793087877787, 11.21024514465928235 ) ) ;
#642 = CARTESIAN_POINT ( 'NONE',  ( -9.375578539472099848, 1.533232399700011683, 10.70113791807854220 ) ) ;
#643 = CARTESIAN_POINT ( 'NONE',  ( 4.490180821391514421, -8.922933199037132113, 9.651137918078598332 ) ) ;
#644 = FACE_OUTER_BOUND ( 'NONE', #6077, .T. ) ;
#645 = CARTESIAN_POINT ( 'NONE',  ( 9.899494936611718643, -9.899494936611608509, 45.00000000000000711 ) ) ;
#646 = CARTESIAN_POINT ( 'NONE',  ( -7.556039541191334585, -11.78653521626503320, 2.289754855340722539 ) ) ;
#647 = ORIENTED_EDGE ( 'NONE', *, *, #769, .T. ) ;
#648 = CARTESIAN_POINT ( 'NONE',  ( -15.44746603149413922, -5.543385399275820191, 12.92453085894499587 ) ) ;
#649 = CARTESIAN_POINT ( 'NONE',  ( -58.00000000000002842, 9.020562075080167263E-17, 13.00000000000001243 ) ) ;
#650 = CARTESIAN_POINT ( 'NONE',  ( -16.30827793483735988, 1.837501619626141780, 29.35714285714285765 ) ) ;
#651 = PLANE ( 'NONE',  #8473 ) ;
#652 = SURFACE_STYLE_FILL_AREA ( #4470 ) ;
#653 = DIRECTION ( 'NONE',  ( -1.000000000000000000, 0.000000000000000000, -0.000000000000000000 ) ) ;
#654 = CARTESIAN_POINT ( 'NONE',  ( 9.865911304835474738, 1.562606840307950051, 10.05000000000002736 ) ) ;
#655 = CARTESIAN_POINT ( 'NONE',  ( 4.270415729527831772, 8.486213763410688671, 13.59886208192144430 ) ) ;
#656 = CARTESIAN_POINT ( 'NONE',  ( -158.0000000000000284, -16.00000000000000355, 0.000000000000000000 ) ) ;
#657 = CARTESIAN_POINT ( 'NONE',  ( -1.837501619626328297, 16.30827793483733856, 48.64285714285716011 ) ) ;
#658 = DIRECTION ( 'NONE',  ( -1.000000000000000000, -1.040834085586086106E-16, -6.090254278793936846E-33 ) ) ;
#659 = CARTESIAN_POINT ( 'NONE',  ( -8.621071003556675549, 13.96533075980314642, 16.21832628391214470 ) ) ;
#660 = CARTESIAN_POINT ( 'NONE',  ( -1.791431617652833763, -15.89939535829188877, 15.85714285714286120 ) ) ;
#661 = DIRECTION ( 'NONE',  ( -1.000000000000000000, -0.000000000000000000, -0.000000000000000000 ) ) ;
#662 = EDGE_LOOP ( 'NONE', ( #7898, #847, #3202, #5619 ) ) ;
#663 = CARTESIAN_POINT ( 'NONE',  ( 4.766900247265192903, 9.355568503977902850, 18.60000000000000497 ) ) ;
#664 = EDGE_LOOP ( 'NONE', ( #485, #1187 ) ) ;
#665 = CARTESIAN_POINT ( 'NONE',  ( -15.89939535829186923, -1.791431617653016062, 41.14285714285714590 ) ) ;
#666 = FILL_AREA_STYLE ('',( #8623 ) ) ;
#667 = CARTESIAN_POINT ( 'NONE',  ( -9.333916720356675967, -4.809394265263096990, 6.398862081921446787 ) ) ;
#668 = CARTESIAN_POINT ( 'NONE',  ( 8.512513224245308763, 13.54758718765259040, 1.285714285714285809 ) ) ;
#669 = CARTESIAN_POINT ( 'NONE',  ( -13.89598863503046111, 8.731428362939027465, 5.785714285714282035 ) ) ;
#670 = CARTESIAN_POINT ( 'NONE',  ( -1.567502665446231180, -13.91197093850540334, 27.85714285714285765 ) ) ;
#671 = CARTESIAN_POINT ( 'NONE',  ( 7.556039541191335474, 11.78653521626503320, 29.28975485534071765 ) ) ;
#672 = CARTESIAN_POINT ( 'NONE',  ( -9.865911304835474738, -1.562606840307925626, 11.54999999999998295 ) ) ;
#673 = ORIENTED_EDGE ( 'NONE', *, *, #6657, .T. ) ;
#674 = CARTESIAN_POINT ( 'NONE',  ( -7.340858601237953529, -11.92174236212700222, 42.28167371608785174 ) ) ;
#675 = AXIS2_PLACEMENT_3D ( 'NONE', #8769, #866, #81 ) ;
#676 = ORIENTED_EDGE ( 'NONE', *, *, #3604, .T. ) ;
#677 = CARTESIAN_POINT ( 'NONE',  ( -5.986002070941133901, -13.58603705635637304, -1.270000000000007123 ) ) ;
#678 = CARTESIAN_POINT ( 'NONE',  ( 15.14410076328353227, -5.164528828830166063, 22.56738800180214000 ) ) ;
#679 = CIRCLE ( 'NONE', #4292, 15.00000000000000000 ) ;
#680 = CARTESIAN_POINT ( 'NONE',  ( -5.420364854931998266, -15.49051278174643898, 4.071428571428569398 ) ) ;
#681 = CARTESIAN_POINT ( 'NONE',  ( -4.579542530753125895, 8.877401133907090625, 7.148862081921437017 ) ) ;
#682 = CARTESIAN_POINT ( 'NONE',  ( -15.44746603149413922, -5.543385399275820191, 24.92453085894499765 ) ) ;
#683 = DIRECTION ( 'NONE',  ( 0.000000000000000000, -6.338944243255235518E-49, 1.000000000000000000 ) ) ;
#684 = CARTESIAN_POINT ( 'NONE',  ( 1.595456901104624459, -10.37818827243065201, 12.80113791807860224 ) ) ;
#685 = LINE ( 'NONE', #2124, #348 ) ;
#686 = CARTESIAN_POINT ( 'NONE',  ( -4.503970704919988854, 13.25633410266674517, 46.43261199819787066 ) ) ;
#687 = AXIS2_PLACEMENT_3D ( 'NONE', #4950, #2617, #5245 ) ;
#688 = VECTOR ( 'NONE', #1379, 1000.000000000000000 ) ;
#689 = AXIS2_PLACEMENT_3D ( 'NONE', #1610, #4761, #212 ) ;
#690 = EDGE_LOOP ( 'NONE', ( #3078, #6347, #4247, #9769 ) ) ;
#691 = CARTESIAN_POINT ( 'NONE',  ( -13.89774397934249706, -1.693770420379375974, 7.138816573230711171 ) ) ;
#692 = CARTESIAN_POINT ( 'NONE',  ( 4.766900247265192903, 9.355568503977911732, 6.599999999999994316 ) ) ;
#693 = CARTESIAN_POINT ( 'NONE',  ( -11.31370849898482156, 11.31370849898469544, 30.00000000000000355 ) ) ;
#694 = CYLINDRICAL_SURFACE ( 'NONE', #5832, 18.00000000000002132 ) ;
#695 = VECTOR ( 'NONE', #3899, 1000.000000000000000 ) ;
#696 = CARTESIAN_POINT ( 'NONE',  ( -13.51115193377584589, -4.865839792409295761, 30.92453085894499765 ) ) ;
#697 = CARTESIAN_POINT ( 'NONE',  ( -7.390897758835869524, 7.458344646081644491, 8.001137918078546463 ) ) ;
#698 = CARTESIAN_POINT ( 'NONE',  ( 9.873755945037075321, 1.513077731353043243, 3.051137918078546285 ) ) ;
#699 = CARTESIAN_POINT ( 'NONE',  ( -166.0761157388880918, -1.866610437352971719, 12.86553408738820714 ) ) ;
#700 = CARTESIAN_POINT ( 'NONE',  ( 4.503970704919991519, -13.25633410266674517, 7.432611998197861780 ) ) ;
#701 = CARTESIAN_POINT ( 'NONE',  ( 1.693770420379222319, 13.89774397934251837, -1.138816573230706286 ) ) ;
#702 = ORIENTED_EDGE ( 'NONE', *, *, #2541, .T. ) ;
#703 = CARTESIAN_POINT ( 'NONE',  ( -11.40355824106246807, 11.22385875690704715, 13.99595943037356527 ) ) ;
#704 = CYLINDRICAL_SURFACE ( 'NONE', #8270, 8.000000000000000000 ) ;
#705 = CARTESIAN_POINT ( 'NONE',  ( 13.54758718765249803, 8.512513224245457977, 37.71428571428571530 ) ) ;
#706 = CARTESIAN_POINT ( 'NONE',  ( 13.61000000000001720, 0.000000000000000000, 0.000000000000000000 ) ) ;
#707 = PLANE ( 'NONE',  #2637 ) ;
#708 = CARTESIAN_POINT ( 'NONE',  ( 6.717514421272239744, -6.717514421272154479, 7.500000000000007105 ) ) ;
#709 = CARTESIAN_POINT ( 'NONE',  ( -6.717514421272238856, 6.717514421272181124, 0.000000000000000000 ) ) ;
#710 = CARTESIAN_POINT ( 'NONE',  ( 11.48991645990273724, -11.34085470199652512, -1.270000000000007123 ) ) ;
#711 = CARTESIAN_POINT ( 'NONE',  ( 11.31370849898482334, -11.31370849898469366, 39.00000000000000000 ) ) ;
#712 = CARTESIAN_POINT ( 'NONE',  ( -5.164528828830334817, 15.14410076328347543, 16.43261199819786356 ) ) ;
#713 = CARTESIAN_POINT ( 'NONE',  ( -11.60466159355861926, -11.60466159355875249, 22.50000000000000000 ) ) ;
#714 = DIRECTION ( 'NONE',  ( 1.000000000000000000, 4.755747939841215952E-17, -0.000000000000000000 ) ) ;
#715 = ORIENTED_EDGE ( 'NONE', *, *, #7105, .T. ) ;
#716 = EDGE_CURVE ( 'NONE', #2214, #4164, #4775, .T. ) ;
#717 = CARTESIAN_POINT ( 'NONE',  ( 10.37072757624895836, -1.642561882922356498, 16.19999999999999218 ) ) ;
#718 = CARTESIAN_POINT ( 'NONE',  ( -13.89598863503045933, 8.731428362939027465, 47.78571428571429891 ) ) ;
#719 = ADVANCED_FACE ( 'NONE', ( #7922, #8553 ), #707, .F. ) ;
#720 = CARTESIAN_POINT ( 'NONE',  ( 7.771249796623105333, 7.842167650704658932, 10.74886208192140913 ) ) ;
#721 = CARTESIAN_POINT ( 'NONE',  ( 5.284464991282756152, -15.10213328493384743, 3.428571428571426605 ) ) ;
#722 = CARTESIAN_POINT ( 'NONE',  ( -8.731428362939189114, 13.89598863503036341, 0.2142857142857168273 ) ) ;
#723 = CARTESIAN_POINT ( 'NONE',  ( 7.448449071214646722, 11.85413878919601594, 31.28571428571428470 ) ) ;
#724 = CARTESIAN_POINT ( 'NONE',  ( 12.08964793087886314, -7.750357176954162597, 36.78975485534072476 ) ) ;
#725 = CARTESIAN_POINT ( 'NONE',  ( 9.383039235653818366, -1.486127417882129986, 7.199999999999984190 ) ) ;
#726 = ORIENTED_EDGE ( 'NONE', *, *, #882, .T. ) ;
#727 = CARTESIAN_POINT ( 'NONE',  ( 13.25633410266679313, -4.503970704919842305, 40.56738800180214355 ) ) ;
#728 = VERTEX_POINT ( 'NONE', #4678 ) ;
#729 = CARTESIAN_POINT ( 'NONE',  ( -108.0000000000000284, 2.204364238465235822E-15, -18.00000000000000355 ) ) ;
#730 = CARTESIAN_POINT ( 'NONE',  ( -11.51250119794888072, -11.69682198916848037, 24.49595943037356705 ) ) ;
#731 = CARTESIAN_POINT ( 'NONE',  ( 1.791431617652837316, 15.89939535829188877, 0.8571428571428549859 ) ) ;
#732 = CARTESIAN_POINT ( 'NONE',  ( -4.579542530753125895, 8.877401133907083519, 13.14886208192146633 ) ) ;
#733 = CARTESIAN_POINT ( 'NONE',  ( 13.47998361472151529, 8.620103694222146729, 21.71024514465928235 ) ) ;
#734 = CARTESIAN_POINT ( 'NONE',  ( 4.766900247265192903, 9.355568503977902850, 0.5999999999999894307 ) ) ;
#735 = CARTESIAN_POINT ( 'NONE',  ( -7.806708723663830618, -7.806708723663901672, 5.250000000000008882 ) ) ;
#736 = DIRECTION ( 'NONE',  ( 0.000000000000000000, 0.000000000000000000, 1.000000000000000000 ) ) ;
#737 = TOROIDAL_SURFACE ( 'NONE', #6796, 3.299999999999999822, 0.2000000000000000111 ) ;
#738 = ORIENTED_EDGE ( 'NONE', *, *, #3509, .T. ) ;
#739 = CARTESIAN_POINT ( 'NONE',  ( 11.22385875690704715, 11.40355824106246985, 51.49595943037355994 ) ) ;
#740 = EDGE_CURVE ( 'NONE', #7778, #3156, #4627, .T. ) ;
#741 = CARTESIAN_POINT ( 'NONE',  ( -1.642561882922479732, 10.37072757624895303, 3.299999999999969624 ) ) ;
#742 = CARTESIAN_POINT ( 'NONE',  ( 13.89598863503046111, -8.731428362939032795, 26.78571428571429536 ) ) ;
#743 = FACE_OUTER_BOUND ( 'NONE', #221, .T. ) ;
#744 = CARTESIAN_POINT ( 'NONE',  ( -1.776620879821455556, -10.89658364409025637, 9.951137918078590161 ) ) ;
#745 = CARTESIAN_POINT ( 'NONE',  ( 6.683790977649321619, -6.751237864895082375, 3.501137918078585987 ) ) ;
#746 = DIRECTION ( 'NONE',  ( 0.000000000000000000, -8.191099868251446680E-34, -1.000000000000000000 ) ) ;
#747 = CARTESIAN_POINT ( 'NONE',  ( 10.13893307789800957, 12.50873118924980609, 47.39553751340654486 ) ) ;
#748 = CARTESIAN_POINT ( 'NONE',  ( -14.25515036105622890, 1.737328882695209575, 9.361183426769292382 ) ) ;
#749 = CARTESIAN_POINT ( 'NONE',  ( 10.24623928997352884, 10.06191849875416899, -0.4959594303735606058 ) ) ;
#750 = EDGE_LOOP ( 'NONE', ( #8233, #3945, #2776, #7235 ) ) ;
#751 = CARTESIAN_POINT ( 'NONE',  ( 11.51250119794888249, 11.69682198916847682, 3.495959430373559940 ) ) ;
#752 = DIRECTION ( 'NONE',  ( -1.000000000000000000, 1.842239752758738928E-31, -1.780435181894459419E-32 ) ) ;
#753 = CARTESIAN_POINT ( 'NONE',  ( 8.512513224245308763, 13.54758718765259040, 43.28571428571429180 ) ) ;
#754 = DIRECTION ( 'NONE',  ( -1.000000000000000000, -0.000000000000000000, -0.000000000000000000 ) ) ;
#755 = EDGE_CURVE ( 'NONE', #7104, #6156, #3859, .T. ) ;
#756 = CARTESIAN_POINT ( 'NONE',  ( 8.486213763410640709, 4.270415729527937465, -0.09886208192143307316 ) ) ;
#757 = CARTESIAN_POINT ( 'NONE',  ( 9.858066664633883036, 1.612135949262858858, 14.04886208192143471 ) ) ;
#758 = DIRECTION ( 'NONE',  ( 1.000000000000000000, -0.000000000000000000, -0.000000000000000000 ) ) ;
#759 = CARTESIAN_POINT ( 'NONE',  ( -8.620103694221995738, -13.47998361472161299, 20.28975485534072121 ) ) ;
#760 = FACE_OUTER_BOUND ( 'NONE', #4497, .T. ) ;
#761 = CARTESIAN_POINT ( 'NONE',  ( 11.22385875690717683, -11.40355824106234373, 19.00404056962642940 ) ) ;
#762 = CARTESIAN_POINT ( 'NONE',  ( 6.903294689124716221, 14.32703841502055830, 48.72999999999998266 ) ) ;
#763 = DIRECTION ( 'NONE',  ( 0.000000000000000000, 0.000000000000000000, 1.000000000000000000 ) ) ;
#764 = CARTESIAN_POINT ( 'NONE',  ( -15.49051278174637858, -5.420364854932175014, 46.92857142857143060 ) ) ;
#765 = PRESENTATION_STYLE_ASSIGNMENT (( #4690 ) ) ;
#766 = CARTESIAN_POINT ( 'NONE',  ( -10.89658364409024749, -1.776620879821561472, 9.548862081921404510 ) ) ;
#767 = CARTESIAN_POINT ( 'NONE',  ( -1.791431617652833763, -15.89939535829188877, 9.857142857142855874 ) ) ;
#768 = CARTESIAN_POINT ( 'NONE',  ( 13.91197093850538380, 1.567502665446386390, 32.14285714285714590 ) ) ;
#769 = EDGE_CURVE ( 'NONE', #9409, #594, #5277, .T. ) ;
#770 = CARTESIAN_POINT ( 'NONE',  ( -13.17239914596754424, 4.743843029824683200, 33.57546914105500946 ) ) ;
#771 = CARTESIAN_POINT ( 'NONE',  ( 1.486127417882244783, -9.383039235653782839, 7.800000000000029132 ) ) ;
#772 = CARTESIAN_POINT ( 'NONE',  ( 4.724406229267374968, 9.377220287599055126, 1.598862081921434308 ) ) ;
#773 = CARTESIAN_POINT ( 'NONE',  ( 14.26974319298268767, -1.607813917172876916, 2.357142857142856762 ) ) ;
#774 = ORIENTED_EDGE ( 'NONE', *, *, #1414, .F. ) ;
#775 = CYLINDRICAL_SURFACE ( 'NONE', #4084, 3.632200000000000539 ) ;
#776 = CARTESIAN_POINT ( 'NONE',  ( -1.665163862719845067, -15.91362231745477374, 23.85310228751642825 ) ) ;
#777 = CARTESIAN_POINT ( 'NONE',  ( 5.284464991282756152, -15.10213328493384743, 3.428571428571426605 ) ) ;
#778 = CARTESIAN_POINT ( 'NONE',  ( -15.88516839912898071, -1.917699372586004980, 19.13881657323070584 ) ) ;
#779 = CARTESIAN_POINT ( 'NONE',  ( -5.012215536711506658, 9.837026868206027785, 3.149999999999957723 ) ) ;
#780 = CARTESIAN_POINT ( 'NONE',  ( 4.766900247265192903, 9.355568503977911732, 6.599999999999994316 ) ) ;
#781 = FACE_OUTER_BOUND ( 'NONE', #3740, .T. ) ;
#782 = AXIS2_PLACEMENT_3D ( 'NONE', #4977, #2444, #8966 ) ;
#783 = CARTESIAN_POINT ( 'NONE',  ( -1.791431617652833763, -15.89939535829188877, 33.85714285714285410 ) ) ;
#784 = ORIENTED_EDGE ( 'NONE', *, *, #8505, .T. ) ;
#785 = CARTESIAN_POINT ( 'NONE',  ( 7.750357176954296712, -12.08964793087877787, 5.210245144659280569 ) ) ;
#786 = CARTESIAN_POINT ( 'NONE',  ( -1.727091770866549414, -10.90442828429184807, 1.949999999999996403 ) ) ;
#787 = CARTESIAN_POINT ( 'NONE',  ( 15.49051278174638036, 5.420364854932175014, 13.92857142857143238 ) ) ;
#788 = CARTESIAN_POINT ( 'NONE',  ( 56.99999999999997158, 0.000000000000000000, 8.000000000000000000 ) ) ;
#789 = SHAPE_REPRESENTATION ( 'main cylinder', ( #3995 ), #10094 ) ;
#790 = CARTESIAN_POINT ( 'NONE',  ( 4.967534682030706250, -9.859792900771042312, 3.651137918078570355 ) ) ;
#791 = CARTESIAN_POINT ( 'NONE',  ( -7.098671581784199880, -7.027753727702809705, 13.25113791807857311 ) ) ;
#792 = CARTESIAN_POINT ( 'NONE',  ( -166.4202771397491176, -1.620148664718404685, 12.89903195109847545 ) ) ;
#793 = CARTESIAN_POINT ( 'NONE',  ( 9.809645194534072132, -9.989344678689256796, 7.004040569626434731 ) ) ;
#794 = CARTESIAN_POINT ( 'NONE',  ( 13.59724543428031573, 4.619798703722006294, 17.93261199819786711 ) ) ;
#795 = ORIENTED_EDGE ( 'NONE', *, *, #5893, .F. ) ;
#796 = CARTESIAN_POINT ( 'NONE',  ( -11.40355824106246807, 11.22385875690704715, 7.995959430373565269 ) ) ;
#797 = CARTESIAN_POINT ( 'NONE',  ( 2.000000000000001776, 1.329782007511007169, 0.7677499999999559677 ) ) ;
#798 = CARTESIAN_POINT ( 'NONE',  ( 1.791431617652837316, 15.89939535829188877, 42.85714285714285410 ) ) ;
#799 = AXIS2_PLACEMENT_3D ( 'NONE', #9882, #2785, #9165 ) ;
#800 = CARTESIAN_POINT ( 'NONE',  ( -5.110041130070070992, -16.97680807127747826, -1.270000000000007123 ) ) ;
#801 = CYLINDRICAL_SURFACE ( 'NONE', #164, 15.99999999999999645 ) ;
#802 = CARTESIAN_POINT ( 'NONE',  ( 7.063212654743467489, 7.063212654743557195, 12.75000000000000533 ) ) ;
#803 = CARTESIAN_POINT ( 'NONE',  ( 8.464561979789474222, 4.312909747525755400, 6.899999999999961275 ) ) ;
#804 = CARTESIAN_POINT ( 'NONE',  ( -15.49051278174638036, -5.420364854932175902, 34.92857142857145192 ) ) ;
#805 = CARTESIAN_POINT ( 'NONE',  ( -5.986002070941136566, -13.58603705635637482, 0.000000000000000000 ) ) ;
#806 = CARTESIAN_POINT ( 'NONE',  ( 1.562606840307832146, 9.865911304835508489, 3.450000000000007283 ) ) ;
#807 = CARTESIAN_POINT ( 'NONE',  ( 15.91362231745475597, 1.665163862720026255, 36.14689771248357886 ) ) ;
#808 = EDGE_LOOP ( 'NONE', ( #8183, #7478, #5542, #1198 ) ) ;
#809 = CARTESIAN_POINT ( 'NONE',  ( 5.420364854932001819, 15.49051278174644430, 19.07142857142856940 ) ) ;
#810 = CARTESIAN_POINT ( 'NONE',  ( 0.000000000000000000, 5.592146987065130084E-32, 0.000000000000000000 ) ) ;
#811 = CARTESIAN_POINT ( 'NONE',  ( -1.791431617652833763, -15.89939535829188877, 3.857142857142857650 ) ) ;
#812 = CARTESIAN_POINT ( 'NONE',  ( -170.0000000000000284, -13.00000000000001066, 1.592040838891559687E-15 ) ) ;
#813 = UNCERTAINTY_MEASURE_WITH_UNIT (LENGTH_MEASURE( 1.000000000000000082E-05 ), #5110, 'distance_accuracy_value', 'NONE');
#814 = CARTESIAN_POINT ( 'NONE',  ( -10.89658364409024749, -1.776620879821559917, 6.548862081921412504 ) ) ;
#815 = CARTESIAN_POINT ( 'NONE',  ( -9.809645194534070356, 9.989344678689256796, 46.00404056962644006 ) ) ;
#816 = CARTESIAN_POINT ( 'NONE',  ( 16.30827793483735633, -1.837501619626142890, 14.35714285714285587 ) ) ;
#817 = CARTESIAN_POINT ( 'NONE',  ( -7.448449071214644945, -11.85413878919601771, 40.28571428571428470 ) ) ;
#818 = CARTESIAN_POINT ( 'NONE',  ( 10.24623928997352884, 10.06191849875416899, 29.50404056962643295 ) ) ;
#819 = CARTESIAN_POINT ( 'NONE',  ( 4.312909747525650594, 8.464561979789532842, 12.59999999999999964 ) ) ;
#820 = CARTESIAN_POINT ( 'NONE',  ( -10.90442828429183919, -1.727091770866654663, 17.55000000000002913 ) ) ;
#821 = ORIENTED_EDGE ( 'NONE', *, *, #1366, .T. ) ;
#822 = CARTESIAN_POINT ( 'NONE',  ( -9.989344678689363377, 9.809645194533960222, 49.99595943037357415 ) ) ;
#823 = CARTESIAN_POINT ( 'NONE',  ( 0.000000000000000000, 0.000000000000000000, 0.000000000000000000 ) ) ;
#824 = CARTESIAN_POINT ( 'NONE',  ( -8.841785722321695573, 13.82664651025757152, 32.21024514465928235 ) ) ;
#825 = CARTESIAN_POINT ( 'NONE',  ( -11.60466159355861748, -11.60466159355874893, 22.50000000000000355 ) ) ;
#826 = AXIS2_PLACEMENT_3D ( 'NONE', #1580, #4054, #7874 ) ;
#827 = CARTESIAN_POINT ( 'NONE',  ( -5.297344310588352201, -15.53355953199867301, 18.06738800180213644 ) ) ;
#828 = CARTESIAN_POINT ( 'NONE',  ( -7.424621202458789426, 7.424621202458724589, 0.000000000000000000 ) ) ;
#829 = CARTESIAN_POINT ( 'NONE',  ( -7.806708723663830618, -7.806708723663906113, 2.249999999999986233 ) ) ;
#830 = CARTESIAN_POINT ( 'NONE',  ( -158.0000000000000284, -6.938893903907228378E-15, 0.000000000000000000 ) ) ;
#831 = SURFACE_STYLE_USAGE ( .BOTH. , #8689 ) ;
#832 = AXIS2_PLACEMENT_3D ( 'NONE', #8024, #7249, #6413 ) ;
#833 = CIRCLE ( 'NONE', #9, 1.649999999999984812 ) ;
#834 = ORIENTED_EDGE ( 'NONE', *, *, #1944, .F. ) ;
#835 = CARTESIAN_POINT ( 'NONE',  ( -13.51115193377584589, -4.865839792409295761, 18.92453085894499409 ) ) ;
#836 = CARTESIAN_POINT ( 'NONE',  ( 5.012215536711512875, -9.837026868206002916, 13.65000000000003411 ) ) ;
#837 = EDGE_CURVE ( 'NONE', #7040, #4031, #8175, .T. ) ;
#838 = CARTESIAN_POINT ( 'NONE',  ( -165.2165827598522867, 1.639280964940008856, 12.89624789671500515 ) ) ;
#839 = CARTESIAN_POINT ( 'NONE',  ( -9.814260835641038128, 5.056896391392221801, 7.851137918078569200 ) ) ;
#841 = AXIS2_PLACEMENT_3D ( 'NONE', #6825, #4314, #6714 ) ;
#840 = CARTESIAN_POINT ( 'NONE',  ( -4.490180821391513533, 8.922933199037158758, 11.15113791807855215 ) ) ;
#842 = AXIS2_PLACEMENT_3D ( 'NONE', #8392, #10108, #4420 ) ;
#843 = CIRCLE ( 'NONE', #1171, 15.44569104238500046 ) ;
#844 = FACE_OUTER_BOUND ( 'NONE', #5304, .T. ) ;
#845 = CARTESIAN_POINT ( 'NONE',  ( 13.59724543428031573, 4.619798703722006294, 11.93261199819786178 ) ) ;
#846 = CARTESIAN_POINT ( 'NONE',  ( -7.556039541191334585, -11.78653521626503320, 8.289754855340721207 ) ) ;
#847 = ORIENTED_EDGE ( 'NONE', *, *, #5286, .T. ) ;
#848 = VECTOR ( 'NONE', #3742, 1000.000000000000114 ) ;
#849 = CIRCLE ( 'NONE', #2646, 8.200000000000009948 ) ;
#850 = DIRECTION ( 'NONE',  ( 1.000000000000000000, 0.000000000000000000, 0.000000000000000000 ) ) ;
#851 = COLOUR_RGB ( '', 0.40784314, 0.44705882, 0.49803922) ;
#852 = CARTESIAN_POINT ( 'NONE',  ( 5.420364854932001819, 15.49051278174644430, 43.07142857142858361 ) ) ;
#853 = DIRECTION ( 'NONE',  ( 0.000000000000000000, 8.191099868251446680E-34, 1.000000000000000000 ) ) ;
#854 = FACE_OUTER_BOUND ( 'NONE', #1961, .T. ) ;
#855 = CARTESIAN_POINT ( 'NONE',  ( 9.383039235653818366, -1.486127417882131097, 13.19999999999998863 ) ) ;
#856 = CARTESIAN_POINT ( 'NONE',  ( -9.865911304835474738, -1.562606840307925626, 2.550000000000035350 ) ) ;
#857 = DIRECTION ( 'NONE',  ( -1.000000000000000000, -0.000000000000000000, -0.000000000000000000 ) ) ;
#858 = CARTESIAN_POINT ( 'NONE',  ( 8.621071003556677326, -13.96533075980314287, 25.21832628391215181 ) ) ;
#859 = CARTESIAN_POINT ( 'NONE',  ( 4.534861676072321046, -8.900167166472098046, 1.650000000000006128 ) ) ;
#860 = COLOUR_RGB ( '', 0.31764706, 0.68627451, 0.89019608) ;
#861 = CARTESIAN_POINT ( 'NONE',  ( 1.707986654103998303, -16.32287076676380266, 31.64689771248358241 ) ) ;
#862 = ORIENTED_EDGE ( 'NONE', *, *, #8540, .T. ) ;
#863 = EDGE_CURVE ( 'NONE', #8514, #4989, #4957, .T. ) ;
#864 = CARTESIAN_POINT ( 'NONE',  ( -11.60466159355861926, -11.60466159355875249, 28.50000000000001066 ) ) ;
#865 = DIRECTION ( 'NONE',  ( 1.000000000000000000, 0.000000000000000000, 0.000000000000000000 ) ) ;
#866 = DIRECTION ( 'NONE',  ( 1.000000000000000000, 4.755747939841215952E-17, -0.000000000000000000 ) ) ;
#867 = ADVANCED_FACE ( 'NONE', ( #9741 ), #4252, .F. ) ;
#868 = CIRCLE ( 'NONE', #8955, 18.00000000000000355 ) ;
#869 = CARTESIAN_POINT ( 'NONE',  ( 10.89658364409024749, 1.776620879821587229, 14.04886208192143471 ) ) ;
#870 = CARTESIAN_POINT ( 'NONE',  ( -9.333916720356675967, -4.809394265263096990, 15.39886208192141126 ) ) ;
#871 = CARTESIAN_POINT ( 'NONE',  ( -1.478298951650703019, 14.28433602490913579, 40.64689771248358596 ) ) ;
#872 = CARTESIAN_POINT ( 'NONE',  ( -5.420364854931999155, -15.49051278174644253, 16.07142857142857650 ) ) ;
#873 = ITEM_DEFINED_TRANSFORMATION ( 'NONE', 'NONE', #6712,  #3995 ) ;
#874 = CARTESIAN_POINT ( 'NONE',  ( -12.15899005565164792, 7.639999817571650809, 35.78571428571429180 ) ) ;
#875 = CARTESIAN_POINT ( 'NONE',  ( 11.92174236212692229, 7.340858601238088532, 41.71832628391215536 ) ) ;
#876 = CARTESIAN_POINT ( 'NONE',  ( -7.529642458189277576, 12.22833218042435455, 34.21832628391215536 ) ) ;
#877 = CARTESIAN_POINT ( 'NONE',  ( 7.063212654743468377, 7.063212654743554531, 9.749999999999982236 ) ) ;
#878 = CARTESIAN_POINT ( 'NONE',  ( 10.37072757624895836, -1.642561882922356498, 13.19999999999998863 ) ) ;
#879 = VERTEX_POINT ( 'NONE', #8076 ) ;
#880 = CARTESIAN_POINT ( 'NONE',  ( -1.567502665446231180, -13.91197093850540334, 3.857142857142857650 ) ) ;
#881 = ORIENTED_EDGE ( 'NONE', *, *, #2812, .F. ) ;
#882 = EDGE_CURVE ( 'NONE', #6987, #9116, #2598, .T. ) ;
#883 = DIRECTION ( 'NONE',  ( 1.000000000000000000, 0.000000000000000000, 0.000000000000000000 ) ) ;
#884 = CARTESIAN_POINT ( 'NONE',  ( 1.837501619626329630, -16.30827793483733501, 21.64285714285714590 ) ) ;
#885 = AXIS2_PLACEMENT_3D ( 'NONE', #5887, #6702, #8433 ) ;
#886 = CARTESIAN_POINT ( 'NONE',  ( -13.47998361472151174, -8.620103694222146729, 42.71024514465928235 ) ) ;
#887 = DIRECTION ( 'NONE',  ( 0.000000000000000000, 8.191099868251448390E-34, 1.000000000000000000 ) ) ;
#888 = CARTESIAN_POINT ( 'NONE',  ( -5.012215536711506658, 9.837026868206022456, 6.149999999999980815 ) ) ;
#889 = CARTESIAN_POINT ( 'NONE',  ( -8.787954181158717404, -8.913453481710840620, 0.000000000000000000 ) ) ;
#890 = VECTOR ( 'NONE', #2246, 1000.000000000000000 ) ;
#891 = SURFACE_STYLE_USAGE ( .BOTH. , #7906 ) ;
#892 = ORIENTED_EDGE ( 'NONE', *, *, #7551, .T. ) ;
#893 = CARTESIAN_POINT ( 'NONE',  ( 13.89774397934249706, 1.693770420379375308, 10.13881657323070762 ) ) ;
#894 = CARTESIAN_POINT ( 'NONE',  ( 7.806708723663832394, 7.806708723663926541, 15.74999999999996803 ) ) ;
#895 = CARTESIAN_POINT ( 'NONE',  ( 10.60660171779815464, 10.60660171779826833, 49.50000000000000000 ) ) ;
#896 = CARTESIAN_POINT ( 'NONE',  ( 12.22833218042443271, -7.529642458189144349, 28.78167371608785174 ) ) ;
#897 = CARTESIAN_POINT ( 'NONE',  ( -10.36326688006724162, 1.689666864740236640, 4.701137918078535982 ) ) ;
#898 = CARTESIAN_POINT ( 'NONE',  ( -6.683790977649319842, 6.751237864895094809, 14.00113791807859620 ) ) ;
#899 = DIRECTION ( 'NONE',  ( -1.000000000000000000, 0.000000000000000000, 0.000000000000000000 ) ) ;
#900 = CARTESIAN_POINT ( 'NONE',  ( -13.59724543428031573, -4.619798703722008959, 2.932611998197868886 ) ) ;
#901 = CARTESIAN_POINT ( 'NONE',  ( 7.556039541191335474, 11.78653521626503320, 17.28975485534072121 ) ) ;
#902 = ORIENTED_EDGE ( 'NONE', *, *, #13, .F. ) ;
#903 = ADVANCED_FACE ( 'NONE', ( #1823 ), #1060, .F. ) ;
#904 = DIRECTION ( 'NONE',  ( -0.7071067811865431318, -0.7071067811865519026, 0.000000000000000000 ) ) ;
#905 = CARTESIAN_POINT ( 'NONE',  ( 1.837501619626330074, -16.30827793483733501, 39.64285714285716722 ) ) ;
#906 = CARTESIAN_POINT ( 'NONE',  ( -164.5737606474697543, -1.597621038677511818, 12.90147476577599406 ) ) ;
#907 = CARTESIAN_POINT ( 'NONE',  ( -1.486127417882243895, 9.383039235653816590, 18.29999999999998295 ) ) ;
#908 = CARTESIAN_POINT ( 'NONE',  ( 1.562606840307832368, 9.865911304835510265, 3.450000000000006839 ) ) ;
#909 = DIRECTION ( 'NONE',  ( -1.000000000000000000, -0.000000000000000000, -0.000000000000000000 ) ) ;
#910 = CARTESIAN_POINT ( 'NONE',  ( 15.53355953199861794, 5.297344310588528060, 29.93261199819786356 ) ) ;
#911 = CARTESIAN_POINT ( 'NONE',  ( 4.312909747525650594, 8.464561979789532842, 3.599999999999992095 ) ) ;
#912 = CARTESIAN_POINT ( 'NONE',  ( -15.91362231745475597, -1.665163862720028254, 27.14689771248358241 ) ) ;
#913 = VERTEX_POINT ( 'NONE', #98 ) ;
#914 = CARTESIAN_POINT ( 'NONE',  ( 8.512513224245308763, 13.54758718765259040, 25.28571428571428470 ) ) ;
#915 = CARTESIAN_POINT ( 'NONE',  ( 2.000000000000001776, -1.329782007510979636, 0.7677500000000114788 ) ) ;
#916 = CARTESIAN_POINT ( 'NONE',  ( -15.10213328493390961, 5.284464991282586510, 5.571428571428574728 ) ) ;
#917 = SURFACE_SIDE_STYLE ('',( #131 ) ) ;
#918 = CARTESIAN_POINT ( 'NONE',  ( -7.027753727702738651, -7.098671581784262941, 6.248862081921465084 ) ) ;
#919 = CARTESIAN_POINT ( 'NONE',  ( -9.333916720356675967, -4.809394265263096990, 15.39886208192141126 ) ) ;
#920 = UNCERTAINTY_MEASURE_WITH_UNIT (LENGTH_MEASURE( 1.000000000000000082E-05 ), #9393, 'distance_accuracy_value', 'NONE');
#921 = CARTESIAN_POINT ( 'NONE',  ( -13.61519076058348254, -8.404922754268771001, 2.718326283912150476 ) ) ;
#922 = CARTESIAN_POINT ( 'NONE',  ( 5.284464991282756152, -15.10213328493384743, 21.42857142857142705 ) ) ;
#923 = CARTESIAN_POINT ( 'NONE',  ( -4.742819248065500481, -13.55419868402813499, 40.07142857142857650 ) ) ;
#924 = CARTESIAN_POINT ( 'NONE',  ( 9.809645194534072132, -9.989344678689256796, 37.00404056962644006 ) ) ;
#925 = CARTESIAN_POINT ( 'NONE',  ( 1.567502665446232957, 13.91197093850540156, 12.85714285714285943 ) ) ;
#926 = CYLINDRICAL_SURFACE ( 'NONE', #6587, 17.72919999999999874 ) ;
#927 = CARTESIAN_POINT ( 'NONE',  ( -7.771249796623103556, -7.842167650704634063, 12.24886208192144998 ) ) ;
#928 = VERTEX_POINT ( 'NONE', #4806 ) ;
#929 = CARTESIAN_POINT ( 'NONE',  ( -10.06191849875405531, -10.24623928997363542, 48.49595943037355994 ) ) ;
#930 = ORIENTED_EDGE ( 'NONE', *, *, #4549, .T. ) ;
#931 = CYLINDRICAL_SURFACE ( 'NONE', #9784, 16.00000000000000000 ) ;
#932 = ADVANCED_FACE ( 'NONE', ( #8639, #3149 ), #7183, .T. ) ;
#933 = CARTESIAN_POINT ( 'NONE',  ( 13.89598863503045933, -8.731428362939032795, 14.78571428571429180 ) ) ;
#934 = CARTESIAN_POINT ( 'NONE',  ( -11.40355824106246807, 11.22385875690704715, 37.99595943037355994 ) ) ;
#935 = CARTESIAN_POINT ( 'NONE',  ( 1.727091770866550968, 10.90442828429187294, 12.44999999999995666 ) ) ;
#936 = CARTESIAN_POINT ( 'NONE',  ( -5.012215536711506658, 9.837026868206027785, 9.150000000000003908 ) ) ;
#937 = CARTESIAN_POINT ( 'NONE',  ( 13.91197093850538380, 1.567502665446386390, 2.142857142857140573 ) ) ;
#938 =( NAMED_UNIT ( * ) SI_UNIT ( $, .STERADIAN. ) SOLID_ANGLE_UNIT ( ) );
#939 = ADVANCED_BREP_SHAPE_REPRESENTATION ( '', ( #7077, #3995 ), #5075 ) ;
#940 = EDGE_LOOP ( 'NONE', ( #7377, #9310, #7961 ) ) ;
#941 = CARTESIAN_POINT ( 'NONE',  ( 14.28433602490915000, -1.478298951650544479, 10.35310228751642292 ) ) ;
#942 = CARTESIAN_POINT ( 'NONE',  ( -5.012215536711508435, 9.837026868206027785, 12.14999999999996483 ) ) ;
#943 = CARTESIAN_POINT ( 'NONE',  ( -165.4282927514613277, 1.597095956079517709, 12.90154007871212194 ) ) ;
#944 = CARTESIAN_POINT ( 'NONE',  ( 11.60466159355862104, 11.60466159355875071, 37.50000000000002842 ) ) ;
#945 = CARTESIAN_POINT ( 'NONE',  ( 11.78653521626494793, 7.556039541191463371, 33.71024514465927524 ) ) ;
#946 = CARTESIAN_POINT ( 'NONE',  ( -4.809394265263009061, -9.333916720356718599, 10.10113791807856742 ) ) ;
#947 = CARTESIAN_POINT ( 'NONE',  ( -8.486213763410637156, -4.270415729527911708, 16.40113791807857524 ) ) ;
#948 = DIRECTION ( 'NONE',  ( -1.000000000000000000, -0.000000000000000000, -0.000000000000000000 ) ) ;
#949 = CARTESIAN_POINT ( 'NONE',  ( 12.08964793087886314, -7.750357176954162597, 18.78975485534072121 ) ) ;
#950 = CARTESIAN_POINT ( 'NONE',  ( -4.865839792409144771, -13.51115193377589740, 8.075469141055007682 ) ) ;
#951 = VERTEX_POINT ( 'NONE', #6970 ) ;
#952 = FACE_OUTER_BOUND ( 'NONE', #9929, .T. ) ;
#953 = CARTESIAN_POINT ( 'NONE',  ( 8.404922754268618235, 13.61519076058357491, 3.281673716087854409 ) ) ;
#954 = DIRECTION ( 'NONE',  ( 0.000000000000000000, 6.338944243255235518E-49, -1.000000000000000000 ) ) ;
#955 = CARTESIAN_POINT ( 'NONE',  ( -164.8564506259586153, -2.149904186608886381, 14.84513091884608649 ) ) ;
#956 = CARTESIAN_POINT ( 'NONE',  ( -4.490180821391513533, 8.922933199037158758, -0.8488620819214613977 ) ) ;
#957 = CARTESIAN_POINT ( 'NONE',  ( 1.562606840307832368, 9.865911304835503159, 6.449999999999969091 ) ) ;
#958 = CARTESIAN_POINT ( 'NONE',  ( 2.000000000000001776, -1.329782007510993402, -0.7677500000000114788 ) ) ;
#959 = CARTESIAN_POINT ( 'NONE',  ( -8.621071003556675549, 13.96533075980314642, 28.21832628391215181 ) ) ;
#960 = CARTESIAN_POINT ( 'NONE',  ( 9.865911304835478290, 1.562606840307950273, 1.049999999999966738 ) ) ;
#961 = CARTESIAN_POINT ( 'NONE',  ( 8.621071003556677326, -13.96533075980314287, 31.21832628391215536 ) ) ;
#962 = ORIENTED_EDGE ( 'NONE', *, *, #4366, .T. ) ;
#963 = CARTESIAN_POINT ( 'NONE',  ( 8.512513224245308763, 13.54758718765259040, 37.28571428571429180 ) ) ;
#964 = CARTESIAN_POINT ( 'NONE',  ( 3.284785595323101770, 14.94556295727555906, 6.336793937239290789E-15 ) ) ;
#965 = CARTESIAN_POINT ( 'NONE',  ( 1.837501619626330074, -16.30827793483733501, 3.642857142857144126 ) ) ;
#966 = SURFACE_STYLE_USAGE ( .BOTH. , #8087 ) ;
#967 = EDGE_CURVE ( 'NONE', #1139, #7327, #8083, .T. ) ;
#968 = CARTESIAN_POINT ( 'NONE',  ( 9.390499931835536884, -1.439022436064272270, 11.19886208192145816 ) ) ;
#969 = CARTESIAN_POINT ( 'NONE',  ( -5.056896391392315948, 9.814260835640997271, 19.14886208192144679 ) ) ;
#970 = PRODUCT_DEFINITION_FORMATION_WITH_SPECIFIED_SOURCE ( 'ANY', '', #308, .NOT_KNOWN. ) ;
#971 = CARTESIAN_POINT ( 'NONE',  ( 1.693770420379222319, 13.89774397934251837, 40.86118342676929416 ) ) ;
#972 = CARTESIAN_POINT ( 'NONE',  ( 1.791431617652837316, 15.89939535829188877, 12.85714285714285943 ) ) ;
#973 = CARTESIAN_POINT ( 'NONE',  ( 11.85413878919593422, 7.448449071214774619, 43.71428571428572241 ) ) ;
#974 = CARTESIAN_POINT ( 'NONE',  ( 4.865839792409144771, 13.51115193377589740, 47.07546914105501656 ) ) ;
#975 = CARTESIAN_POINT ( 'NONE',  ( 7.448449071214646722, 11.85413878919601594, 13.28571428571429003 ) ) ;
#976 = CARTESIAN_POINT ( 'NONE',  ( -9.383039235653820143, 1.486127417882154411, 14.69999999999999041 ) ) ;
#977 = CARTESIAN_POINT ( 'NONE',  ( 7.771249796623105333, 7.842167650704658932, 7.748862081921418010 ) ) ;
#978 = ORIENTED_EDGE ( 'NONE', *, *, #8970, .F. ) ;
#979 = CARTESIAN_POINT ( 'NONE',  ( 11.85413878919593422, 7.448449071214774619, 7.714285714285715301 ) ) ;
#980 = ORIENTED_EDGE ( 'NONE', *, *, #1070, .F. ) ;
#981 = DIRECTION ( 'NONE',  ( 0.000000000000000000, -6.338944243255235518E-49, 1.000000000000000000 ) ) ;
#982 = CARTESIAN_POINT ( 'NONE',  ( -5.284464991282755264, 15.10213328493384743, 12.42857142857142705 ) ) ;
#983 = CARTESIAN_POINT ( 'NONE',  ( -15.44746603149413922, -5.543385399275820191, 36.92453085894499765 ) ) ;
#984 = CARTESIAN_POINT ( 'NONE',  ( -9.355568503977838901, -4.766900247265280832, 8.399999999999963052 ) ) ;
#985 = CARTESIAN_POINT ( 'NONE',  ( -1.727091770866549414, -10.90442828429184630, 10.95000000000000462 ) ) ;
#986 = CARTESIAN_POINT ( 'NONE',  ( 1.607813917173037899, -14.26974319298267169, 3.642857142857143238 ) ) ;
#987 = EDGE_CURVE ( 'NONE', #8978, #9666, #1661, .T. ) ;
#988 = CARTESIAN_POINT ( 'NONE',  ( -13.25633410266679313, 4.503970704919840529, 13.56738800180213822 ) ) ;
#989 = CARTESIAN_POINT ( 'NONE',  ( -1.727091770866549414, -10.90442828429184807, 10.95000000000000284 ) ) ;
#990 = CARTESIAN_POINT ( 'NONE',  ( -13.89598863503046111, 8.731428362939027465, 11.78571428571428115 ) ) ;
#991 = FACE_OUTER_BOUND ( 'NONE', #5671, .T. ) ;
#992 = ADVANCED_FACE ( 'NONE', ( #4599 ), #10132, .F. ) ;
#993 = CARTESIAN_POINT ( 'NONE',  ( 7.842167650704563897, 7.771249796623202144, 17.75113791807856245 ) ) ;
#994 = CARTESIAN_POINT ( 'NONE',  ( -4.490180821391513533, 8.922933199037153429, 14.15113791807854327 ) ) ;
#995 = CARTESIAN_POINT ( 'NONE',  ( 2.000000000000001776, -0.8865213383406622683, -1.535500000000078469 ) ) ;
#996 = CARTESIAN_POINT ( 'NONE',  ( -13.17239914596754424, 4.743843029824683200, 21.57546914105500946 ) ) ;
#997 =( NAMED_UNIT ( * ) PLANE_ANGLE_UNIT ( ) SI_UNIT ( $, .RADIAN. ) );
#998 = CARTESIAN_POINT ( 'NONE',  ( 14.25515036105622535, -1.737328882695210241, 12.36118342676929771 ) ) ;
#999 = VERTEX_POINT ( 'NONE', #1504 ) ;
#1000 = CARTESIAN_POINT ( 'NONE',  ( -5.986002070941136566, -13.58603705635637482, -1.270000000000007123 ) ) ;
#1001 = CARTESIAN_POINT ( 'NONE',  ( 8.404922754268618235, 13.61519076058357491, 15.28167371608785174 ) ) ;
#1002 = CARTESIAN_POINT ( 'NONE',  ( 56.99999999999997158, 0.000000000000000000, 0.000000000000000000 ) ) ;
#1003 = CARTESIAN_POINT ( 'NONE',  ( -163.1340397805202542, -1.077317138390382345, 14.96172600814708353 ) ) ;
#1004 = CIRCLE ( 'NONE', #6592, 11.00000000000000355 ) ;
#1005 = AXIS2_PLACEMENT_3D ( 'NONE', #7687, #7878, #1431 ) ;
#1006 = CIRCLE ( 'NONE', #2647, 2.000000000000001776 ) ;
#1007 = CARTESIAN_POINT ( 'NONE',  ( 1.439022436064387511, -9.390499931835512015, 9.801137918078557831 ) ) ;
#1008 = CARTESIAN_POINT ( 'NONE',  ( -9.383039235653820143, 1.486127417882155299, 2.700000000000035705 ) ) ;
#1009 = CARTESIAN_POINT ( 'NONE',  ( 15.06016580658428694, -5.404401153735007846, 36.57546914105501656 ) ) ;
#1010 = CARTESIAN_POINT ( 'NONE',  ( 13.55419868402807992, 4.742819248065648807, 25.92857142857142705 ) ) ;
#1011 = CARTESIAN_POINT ( 'NONE',  ( -1.707986654103994528, 16.32287076676380266, 40.64689771248358596 ) ) ;
#1012 = VECTOR ( 'NONE', #2875, 1000.000000000000000 ) ;
#1013 = AXIS2_PLACEMENT_3D ( 'NONE', #4039, #3151, #6292 ) ;
#1014 = ORIENTED_EDGE ( 'NONE', *, *, #5317, .T. ) ;
#1015 = CARTESIAN_POINT ( 'NONE',  ( -15.10213328493390961, 5.284464991282586510, 35.57142857142857650 ) ) ;
#1016 = CARTESIAN_POINT ( 'NONE',  ( -8.918407633172652282, 10.81660888964814049, -5.255698201876050631E-17 ) ) ;
#1017 = CARTESIAN_POINT ( 'NONE',  ( -16.30827793483735988, 1.837501619626141780, 11.35714285714285943 ) ) ;
#1018 = DIRECTION ( 'NONE',  ( 0.000000000000000000, 6.938893903907221444E-18, 1.000000000000000000 ) ) ;
#1019 = CARTESIAN_POINT ( 'NONE',  ( 6.717514421272239744, -6.717514421272154479, 1.500000000000001332 ) ) ;
#1020 = CARTESIAN_POINT ( 'NONE',  ( 9.858066664633883036, 1.612135949262857526, 2.048862081921423162 ) ) ;
#1021 = COLOUR_RGB ( '', 0.72549020, 0.75294118, 0.79215686) ;
#1022 = UNCERTAINTY_MEASURE_WITH_UNIT (LENGTH_MEASURE( 1.000000000000000082E-05 ), #599, 'distance_accuracy_value', 'NONE');
#1023 = CARTESIAN_POINT ( 'NONE',  ( 13.17239914596754424, -4.743843029824685864, 42.57546914105501656 ) ) ;
#1024 = CARTESIAN_POINT ( 'NONE',  ( -11.31370849898482156, 11.31370849898469544, 36.00000000000000711 ) ) ;
#1025 = CARTESIAN_POINT ( 'NONE',  ( -11.85413878919593422, -7.448449071214776396, 46.71428571428571530 ) ) ;
#1026 = CARTESIAN_POINT ( 'NONE',  ( 13.59724543428031573, 4.619798703722006294, 35.93261199819787066 ) ) ;
#1027 = TOROIDAL_SURFACE ( 'NONE', #1374, 8.000000000000000000, 1.000000000000000888 ) ;
#1028 = STYLED_ITEM ( 'NONE', ( #10063 ), #147 ) ;
#1029 = CARTESIAN_POINT ( 'NONE',  ( 7.639999817571789364, -12.15899005565156266, 15.21428571428571530 ) ) ;
#1030 = CARTESIAN_POINT ( 'NONE',  ( 8.464561979789474222, 4.312909747525755400, 18.90000000000002700 ) ) ;
#1031 = CARTESIAN_POINT ( 'NONE',  ( 5.056896391392317724, -9.814260835640970626, 5.648862081921440570 ) ) ;
#1032 = ORIENTED_EDGE ( 'NONE', *, *, #9471, .F. ) ;
#1033 = CARTESIAN_POINT ( 'NONE',  ( 4.623906867372411078, -13.21436662431711717, 21.42857142857142705 ) ) ;
#1034 = VECTOR ( 'NONE', #9669, 1000.000000000000114 ) ;
#1035 = VERTEX_POINT ( 'NONE', #4037 ) ;
#1036 = DIRECTION ( 'NONE',  ( 1.000000000000000000, 4.755747939841215952E-17, -0.000000000000000000 ) ) ;
#1037 = ADVANCED_FACE ( 'NONE', ( #8531 ), #4657, .T. ) ;
#1038 = CARTESIAN_POINT ( 'NONE',  ( -13.54758718765249625, -8.512513224245459753, 22.71428571428571530 ) ) ;
#1039 = CARTESIAN_POINT ( 'NONE',  ( -8.404922754268618235, -13.61519076058357491, 36.28167371608785174 ) ) ;
#1040 = CARTESIAN_POINT ( 'NONE',  ( -7.424621202458789426, 7.424621202458723701, 9.000000000000007105 ) ) ;
#1041 = CARTESIAN_POINT ( 'NONE',  ( 4.766900247265192903, 9.355568503977902850, 18.60000000000000497 ) ) ;
#1042 = CARTESIAN_POINT ( 'NONE',  ( 4.742819248065502258, 13.55419868402813499, 13.07142857142857117 ) ) ;
#1043 = CARTESIAN_POINT ( 'NONE',  ( -13.89774397934249706, -1.693770420379375974, 13.13881657323070584 ) ) ;
#1044 = EDGE_LOOP ( 'NONE', ( #14, #3815, #5005, #1903, #4389 ) ) ;
#1045 = CARTESIAN_POINT ( 'NONE',  ( 1.642561882922480621, -10.37072757624892638, 13.80000000000003446 ) ) ;
#1046 = CIRCLE ( 'NONE', #1889, 15.99999999999999645 ) ;
#1047 = SHAPE_REPRESENTATION ( 'basic internal retaining ring_ai_B27.1 - NA2-131', ( #3995 ), #7950 ) ;
#1048 = DIRECTION ( 'NONE',  ( -0.7056782240951974261, 0.7056782240951879892, -0.06353336191096842223 ) ) ;
#1049 = CARTESIAN_POINT ( 'NONE',  ( 1.737328882695370558, -14.25515036105620581, 41.63881657323070584 ) ) ;
#1050 = CARTESIAN_POINT ( 'NONE',  ( 10.36326688006723984, -1.689666864740210883, 18.20113791807854398 ) ) ;
#1051 = CARTESIAN_POINT ( 'NONE',  ( 10.36326688006723984, -1.689666864740210883, 9.201137918078538647 ) ) ;
#1052 = DIRECTION ( 'NONE',  ( 0.000000000000000000, 0.000000000000000000, 1.000000000000000000 ) ) ;
#1053 = CARTESIAN_POINT ( 'NONE',  ( -7.556039541191334585, -11.78653521626503320, 14.28975485534072298 ) ) ;
#1054 =( NAMED_UNIT ( * ) SI_UNIT ( $, .STERADIAN. ) SOLID_ANGLE_UNIT ( ) );
#1055 = EDGE_CURVE ( 'NONE', #4850, #4954, #4759, .T. ) ;
#1056 = CARTESIAN_POINT ( 'NONE',  ( -4.865839792409144771, -13.51115193377589740, 20.07546914105500591 ) ) ;
#1057 = DIRECTION ( 'NONE',  ( -0.000000000000000000, -0.000000000000000000, 1.000000000000000000 ) ) ;
#1058 = CARTESIAN_POINT ( 'NONE',  ( 15.88516839912898071, 1.917699372586004092, 16.13881657323070584 ) ) ;
#1059 = CARTESIAN_POINT ( 'NONE',  ( 56.99999999999997158, 0.000000000000000000, 0.000000000000000000 ) ) ;
#1060 = CYLINDRICAL_SURFACE ( 'NONE', #7772, 15.44569104238500046 ) ;
#1061 = EDGE_CURVE ( 'NONE', #4771, #1717, #2795, .T. ) ;
#1062 = CARTESIAN_POINT ( 'NONE',  ( -1.439022436064386845, 9.390499931835526226, 2.301137918078551614 ) ) ;
#1063 = CARTESIAN_POINT ( 'NONE',  ( -9.383039235653820143, 1.486127417882155299, 17.69999999999999218 ) ) ;
#1064 = CARTESIAN_POINT ( 'NONE',  ( -162.8500000000000512, -5.808233196467851957E-15, 13.00000000000000178 ) ) ;
#1065 = CARTESIAN_POINT ( 'NONE',  ( -1.567502665446231180, -13.91197093850540334, 27.85714285714285765 ) ) ;
#1066 = CARTESIAN_POINT ( 'NONE',  ( -13.55419868402807992, -4.742819248065651472, 34.92857142857145192 ) ) ;
#1067 = ORIENTED_EDGE ( 'NONE', *, *, #429, .T. ) ;
#1068 = CIRCLE ( 'NONE', #6816, 8.000000000000000000 ) ;
#1069 = CARTESIAN_POINT ( 'NONE',  ( 3.272017905259138715, 14.35386563642104107, 8.096169431371285764E-17 ) ) ;
#1070 = EDGE_CURVE ( 'NONE', #9896, #4112, #1160, .T. ) ;
#1071 = CARTESIAN_POINT ( 'NONE',  ( -1.791431617652833763, -15.89939535829188877, 21.85714285714286120 ) ) ;
#1072 = CARTESIAN_POINT ( 'NONE',  ( -108.0000000000000284, 0.000000000000000000, 0.000000000000000000 ) ) ;
#1073 = DIRECTION ( 'NONE',  ( -1.000000000000000000, 1.842239752758738928E-31, -1.780435181894459419E-32 ) ) ;
#1074 = CARTESIAN_POINT ( 'NONE',  ( 1.533232399700100945, -9.375578539472067874, 17.79886208192143471 ) ) ;
#1075 = CARTESIAN_POINT ( 'NONE',  ( 9.333916720356675967, 4.809394265263123636, 13.89886208192141126 ) ) ;
#1076 = ADVANCED_FACE ( 'NONE', ( #2329 ), #5267, .T. ) ;
#1077 = CARTESIAN_POINT ( 'NONE',  ( 8.620103694221997515, 13.47998361472160767, 11.28975485534071943 ) ) ;
#1078 = CARTESIAN_POINT ( 'NONE',  ( -5.284464991282755264, 15.10213328493384743, 30.42857142857143060 ) ) ;
#1079 = CARTESIAN_POINT ( 'NONE',  ( 0.000000000000000000, 0.000000000000000000, 0.000000000000000000 ) ) ;
#1080 = CARTESIAN_POINT ( 'NONE',  ( -1.917699372585823570, -15.88516839912900558, 7.861183426769288829 ) ) ;
#1081 = CARTESIAN_POINT ( 'NONE',  ( 10.15407889436379030, 10.15407889436390576, 7.500000000000005329 ) ) ;
#1082 = CYLINDRICAL_SURFACE ( 'NONE', #9749, 18.00000000000000355 ) ;
#1083 = CARTESIAN_POINT ( 'NONE',  ( -10.37818827243067688, 1.595456901104523428, 9.698862081921454603 ) ) ;
#1084 = ORIENTED_EDGE ( 'NONE', *, *, #1371, .T. ) ;
#1085 = CARTESIAN_POINT ( 'NONE',  ( -14.26974319298268767, 1.607813917172874918, 23.35714285714286476 ) ) ;
#1086 = ORIENTED_EDGE ( 'NONE', *, *, #4434, .F. ) ;
#1087 = CARTESIAN_POINT ( 'NONE',  ( 5.420364854932000931, 15.49051278174644075, 25.07142857142857650 ) ) ;
#1088 = CARTESIAN_POINT ( 'NONE',  ( -15.88516839912898071, -1.917699372586004980, 37.13881657323070584 ) ) ;
#1089 = CARTESIAN_POINT ( 'NONE',  ( 10.37072757624895836, -1.642561882922355609, 7.199999999999984190 ) ) ;
#1090 = CARTESIAN_POINT ( 'NONE',  ( -1.607813917173034124, 14.26974319298267346, 6.642857142857143238 ) ) ;
#1091 = ADVANCED_FACE ( 'NONE', ( #6123 ), #9299, .T. ) ;
#1092 = ORIENTED_EDGE ( 'NONE', *, *, #549, .F. ) ;
#1093 = CARTESIAN_POINT ( 'NONE',  ( 4.619798703721856192, 13.59724543428036725, 33.06738800180213644 ) ) ;
#1094 = CARTESIAN_POINT ( 'NONE',  ( -58.00000000000002132, 5.689893001204698381E-17, 8.200000000000009948 ) ) ;
#1095 = DIRECTION ( 'NONE',  ( -0.8571673007021101132, 1.049727191138615984E-16, 0.5150380749100580413 ) ) ;
#1096 = CARTESIAN_POINT ( 'NONE',  ( 13.89774397934249706, 1.693770420379375308, 34.13881657323070584 ) ) ;
#1097 = CARTESIAN_POINT ( 'NONE',  ( -4.809394265263009061, -9.333916720356716823, 16.10113791807856742 ) ) ;
#1098 = CARTESIAN_POINT ( 'NONE',  ( 10.91227292449344155, 1.677562661911773390, 3.051137918078546285 ) ) ;
#1099 = DIRECTION ( 'NONE',  ( -1.000000000000000000, -0.000000000000000000, -0.000000000000000000 ) ) ;
#1100 = CARTESIAN_POINT ( 'NONE',  ( -9.809645194534070356, 9.989344678689256796, 22.00404056962643651 ) ) ;
#1101 = SURFACE_STYLE_USAGE ( .BOTH. , #1873 ) ;
#1102 = CARTESIAN_POINT ( 'NONE',  ( -9.809645194534070356, 9.989344678689256796, 28.00404056962643651 ) ) ;
#1103 = CARTESIAN_POINT ( 'NONE',  ( -9.355568503977838901, -4.766900247265279944, 11.39999999999996660 ) ) ;
#1104 = CARTESIAN_POINT ( 'NONE',  ( -13.96533075980324234, 8.621071003556515677, 43.78167371608784464 ) ) ;
#1105 = CARTESIAN_POINT ( 'NONE',  ( -0.9960085134059654122, 15.98222653422240747, 48.73000000000000398 ) ) ;
#1106 = CARTESIAN_POINT ( 'NONE',  ( 13.54758718765249803, 8.512513224245457977, 19.71428571428571175 ) ) ;
#1107 = CARTESIAN_POINT ( 'NONE',  ( 11.51250119794888249, 11.69682198916847682, 9.495959430373563492 ) ) ;
#1108 = CARTESIAN_POINT ( 'NONE',  ( -83.00000000000001421, 0.000000000000000000, 0.000000000000000000 ) ) ;
#1109 = CARTESIAN_POINT ( 'NONE',  ( -165.5555415711045839, -2.081714733226260439, 14.85487199390593283 ) ) ;
#1110 = CARTESIAN_POINT ( 'NONE',  ( -9.873755945037078874, -1.513077731353019706, 4.551137918078585365 ) ) ;
#1111 = CARTESIAN_POINT ( 'NONE',  ( 9.383039235653818366, -1.486127417882131097, 13.19999999999998863 ) ) ;
#1112 = DIRECTION ( 'NONE',  ( 1.000000000000000000, 0.000000000000000000, 0.000000000000000000 ) ) ;
#1113 = CARTESIAN_POINT ( 'NONE',  ( -1.607813917173034124, 14.26974319298267524, 36.64285714285714590 ) ) ;
#1114 = VECTOR ( 'NONE', #4151, 1000.000000000000114 ) ;
#1115 = CARTESIAN_POINT ( 'NONE',  ( 13.21436662431716869, -4.623906867372263640, 38.57142857142857650 ) ) ;
#1116 = ORIENTED_EDGE ( 'NONE', *, *, #9269, .T. ) ;
#1117 = CARTESIAN_POINT ( 'NONE',  ( 11.31370849898469899, 11.31370849898481978, 49.50000000000000711 ) ) ;
#1118 = CARTESIAN_POINT ( 'NONE',  ( -165.0000000000000284, -1.734723475976807094E-15, 3.000000000000002665 ) ) ;
#1119 = CARTESIAN_POINT ( 'NONE',  ( -5.420364854931999155, -15.49051278174644253, 10.07142857142856940 ) ) ;
#1120 = CARTESIAN_POINT ( 'NONE',  ( 9.858066664633883036, 1.612135949262857526, 17.04886208192142760 ) ) ;
#1121 = CARTESIAN_POINT ( 'NONE',  ( -8.922933199037192509, 4.490180821391428267, 9.848862081921437195 ) ) ;
#1122 =( BOUNDED_SURFACE ( )  B_SPLINE_SURFACE ( 3, 2, ( 
 ( #7735, #4471, #7626, #546, #6163, #10051, #2910, #6828, #9339, #1376, #4527, #2963, #6882, #1262, #7570, #491, #3637, #6771, #9184, #2089, #8327, #5123, #473, #319, #8963, #7549, #2693, #5883, #5222, #9062, #5986, #6698, #1970, #1921, #6652, #1245, #4295, #8275, #9167, #6603, #2072, #5935, #9835, #2020, #5835, #9114, #5178, #9790, #5023, #376, #8376, #3615, #1196, #8167, #4400, #4347, #7500, #272, #6750, #3418, #3466, #9938, #2843, #1298, #424, #7349, #9012, #1875, #5069, #6554, #8220, #9737, #3568, #9884, #2639, #5788, #1103, #4245, #2786, #7397, #1147, #7449, #3527, #2738, #3677, #2318, #8787, #7607, #878, #5471, #3199, #41, #9987, #4451, #4510, #527, #5520, #1650, #4797, #1552, #8729, #7951, #2127, #9563, #9213, #2420, #6334, #6862, #7665, #10174, #7895, #4750, #8630, #9408, #4030, #3090, #6231, #820, #4699, #7846, #2467, #7174, #1601, #91, #3246, #7064, #5568, #2368, #6384, #581, #6037 ),
 ( #6281, #5618, #3974, #9466, #772, #3920, #6810, #9555, #8679, #2893, #3727, #5268, #9514, #3137, #8429, #7125, #1355, #9766, #4125, #9619, #4951, #9816, #5051, #3398, #4225, #5002, #2521, #8148, #4274, #9713, #8102, #1031, #1128, #7425, #6533, #8048, #8838, #6582, #4177, #9665, #4075, #2618, #1751, #5763, #3352, #977, #7274, #4900, #5670, #7374, #8991, #3501, #3443, #8196, #353, #6632, #200, #2717, #1083, #7999, #6487, #5861, #7326, #3295, #249, #1704, #4849, #7224, #2573, #8935, #1852, #1902, #301, #6436, #2670, #927, #142, #5815, #5715, #8884, #1797, #3238, #1791, #3391, #83, #4019, #1075, #869, #4170, #4942, #8775, #9554, #1697, #9658, #6478, #7214, #919, #242, #4841, #7992, #2566, #135, #4068, #4215, #2610, #3344, #8924, #4995, #8831, #7318, #4118, #9703, #2460, #7939, #6525, #3286, #4893, #7367, #8040, #8140, #5707, #969, #6428, #5663, #5755, #9610, #7264, #293, #5608, #6325, #8091 ),
 ( #7164, #2514, #191, #1742, #6376, #1841, #8877, #1020, #9507, #2411, #5559, #8719, #1641, #4786, #8394, #9904, #1319, #6573, #2757, #397, #5808, #5197, #7629, #6623, #8345, #7521, #1991, #7415, #6669, #1941, #3436, #5146, #6720, #1167, #4319, #9756, #1218, #2710, #9853, #3639, #8297, #5044, #2040, #2661, #8983, #9080, #1264, #493, #343, #7469, #4473, #1895, #3543, #9808, #5905, #6774, #6008, #2091, #8189, #1121, #4267, #4369, #3493, #5853, #9030, #9959, #5091, #445, #8239, #3586, #2811, #5957, #9137, #4422, #7572, #2862, #9186, #5240, #6940, #10110, #7787, #8609, #5352, #4730, #655, #3071, #548, #757, #1378, #9231, #7829, #6884, #3804, #9446, #10004, #4529, #3748, #7686, #2352, #4580, #8504, #2965, #5502, #10207, #8451, #6113, #2250, #3022, #602, #1532, #9341, #10053, #9291, #4681, #6165, #5294, #5397, #1430, #8661, #6997, #1582, #3696, #8555, #7737, #2912, #2303, #6830, #2204, #5448, #4629, #1481 ),
 ( #709, #3856, #10157, #6214, #6056, #9390, #3904, #7048, #3120, #6261, #2147, #4931, #9691, #9647, #4156, #6513, #2600, #856, #1008, #4107, #3951, #2449, #3380, #908, #9495, #122, #5743, #7305, #3178, #5549, #1733, #24, #2553, #1828, #4008, #5697, #4882, #6415, #1630, #4056, #6364, #7876, #9594, #957, #5595, #8758, #803, #5650, #7155, #73, #7926, #8708, #174, #8078, #8912, #8865, #227, #7097, #6314, #3227, #2400, #7251, #4777, #1685, #9542, #7203, #4828, #3274, #7981, #2501, #8819, #8026, #3332, #6469, #1778, #9842, #6562, #3573, #9174, #8129, #382, #6707, #2026, #8972, #5842, #2850, #5995, #5077, #1111, #1929, #5184, #7557, #3622, #3424, #9945, #4983, #9020, #7356, #1884, #4255, #8333, #4204, #1154, #7404, #5890, #9069, #8227, #4305, #7456, #9891, #3534, #1251, #6659, #2745, #1977, #5135, #2794, #9797, #1063, #8282, #7507, #279, #4408, #5797, #9742, #480, #328, #1204, #6759, #2649, #5032 ),
 ( #5944, #3477, #9124, #8177, #6610, #2701, #4355, #432, #5434, #3792, #4616, #5384, #2899, #8544, #4667, #10097, #5338, #8493, #1520, #7818, #6922, #8439, #9219, #6982, #5228, #5276, #8593, #698, #3845, #9328, #745, #1363, #3684, #4516, #3058, #589, #10145, #3008, #2238, #1305, #2080, #6202, #6819, #1467, #3892, #9377, #7771, #2134, #1419, #4457, #10040, #6251, #8382, #7036, #2952, #2291, #10196, #7614, #535, #7673, #9993, #6152, #3111, #3734, #6043, #6870, #6096, #9277, #2191, #4569, #7723, #643, #1619, #2388, #4767, #2485, #9580, #61, #3998, #3317, #7913, #840, #5639, #3217, #7143, #7294, #5686, #6404, #1766, #8066, #1669, #160, #7192, #2540, #5538, #791, #9636, #6353, #7968, #217, #898, #994, #8806, #4046, #9532, #8746, #6457, #2437, #109, #4143, #8697, #3368, #8015, #4818, #4093, #5583, #947, #7242, #3262, #7085, #1724, #9428, #8856, #4870, #4921, #2339, #7, #5491, #8649, #1572, #4718 ),
 ( #7864, #6302, #3941, #3164, #9485, #8901, #7444, #6550, #4289, #8163, #2634, #7344, #1192, #371, #3520, #9682, #4342, #9733, #8121, #6694, #1869, #5065, #4396, #8213, #5174, #5879, #1143, #1098, #5830, #7495, #3458, #6648, #8324, #5782, #1242, #5115, #9006, #421, #5017, #8269, #3564, #8957, #4195, #9786, #7545, #9879, #9833, #9057, #2733, #267, #1965, #9109, #2783, #2687, #1917, #5931, #2017, #471, #4239, #3414, #6502, #2589, #7390, #1815, #5734, #317, #4972, #6600, #1051, #4448, #8532, #1407, #4560, #6743, #1458, #9936, #6806, #6971, #2230, #5376, #632, #10133, #2889, #5219, #6031, #4608, #2123, #7759, #7711, #3780, #2839, #3612, #684, #8371, #6912, #2278, #3833, #10082, #524, #10031, #5983, #1351, #7810, #9162, #3049, #4506, #6191, #9317, #2069, #1292, #3672, #7599, #2998, #9366, #9983, #5425, #8582, #9211, #5263, #1505, #8423, #4658, #7660, #578, #3723, #6859, #6141, #2942, #6085, #9262, #2184 ),
 ( #5327, #8483, #3208, #9571, #6342, #4081, #7134, #50, #9522, #1561, #8794, #2428, #8640, #4707, #1714, #829, #5479, #5574, #8687, #5679, #7184, #8848, #3883, #8737, #7904, #3100, #2474, #4909, #3930, #5628, #4807, #1657, #7856, #3985, #9476, #735, #7958, #4038, #1609, #4760, #7026, #888, #3772, #3150, #780, #7074, #3253, #8006, #2530, #4859, #7231, #9627, #1758, #6290, #151, #99, #10184, #5528, #6447, #6393, #2330, #936, #6240, #3306, #9418, #2377, #2042, #1220, #8395, #2813, #9673, #6777, #2148, #985, #3588, #9960, #5241, #1805, #8946, #6057, #9232, #8298, #4185, #5148, #1320, #550, #6831, #6495, #2913, #8055, #1859, #210, #4960, #7335, #4474, #7286, #4370, #259, #9138, #5198, #7523, #446, #6721, #2863, #9906, #7630, #5959, #8347, #1265, #4424, #6009, #2625, #4134, #7573, #495, #3360, #3697, #8893, #2582, #10005, #3406, #3640, #5725, #8112, #1041, #6542, #9721, #5771, #9187, #2092, #7738 ) ),
 .UNSPECIFIED., .T., .F., .F. ) 
 B_SPLINE_SURFACE_WITH_KNOTS ( ( 4, 3, 4 ),
 ( 3, 2, 2, 2, 2, 2, 2, 2, 2, 2, 2, 2, 2, 2, 2, 2, 2, 2, 2, 2, 2, 2, 2, 2, 2, 2, 2, 2, 2, 2, 2, 2, 2, 2, 2, 2, 2, 2, 2, 2, 2, 2, 2, 2, 2, 2, 2, 2, 2, 2, 2, 2, 2, 2, 2, 2, 2, 2, 2, 2, 2, 2, 2, 2, 2, 3 ),
 ( 0.000000000000000000, 0.5000000000000000000, 1.000000000000000000 ),
 ( 0.000000000000000000, 0.01428571428571428527, 0.02857142857142857054, 0.04285714285714285754, 0.05714285714285714107, 0.07142857142857142461, 0.08571428571428571508, 0.1000000000000000056, 0.1142857142857142821, 0.1285714285714285587, 0.1428571428571428492, 0.1571428571428571397, 0.1714285714285714302, 0.1857142857142857206, 0.2000000000000000111, 0.2142857142857142738, 0.2285714285714285643, 0.2428571428571428548, 0.2571428571428571175, 0.2714285714285714080, 0.2857142857142856984, 0.2999999999999999889, 0.3142857142857142794, 0.3285714285714285698, 0.3428571428571428603, 0.3571428571428571508, 0.3714285714285714413, 0.3857142857142857317, 0.4000000000000000222, 0.4142857142857143127, 0.4285714285714285476, 0.4428571428571428381, 0.4571428571428571286, 0.4714285714285714191, 0.4857142857142857095, 0.5000000000000000000, 0.5142857142857142350, 0.5285714285714285809, 0.5428571428571428159, 0.5571428571428571619, 0.5714285714285713969, 0.5857142857142857428, 0.5999999999999999778, 0.6142857142857143238, 0.6285714285714285587, 0.6428571428571429047, 0.6571428571428571397, 0.6714285714285713746, 0.6857142857142857206, 0.6999999999999999556, 0.7142857142857143016, 0.7285714285714285365, 0.7428571428571428825, 0.7571428571428571175, 0.7714285714285714635, 0.7857142857142856984, 0.8000000000000000444, 0.8142857142857142794, 0.8285714285714286254, 0.8428571428571428603, 0.8571428571428570953, 0.8714285714285714413, 0.8857142857142856762, 0.9000000000000000222, 0.9142857142857142572, 0.9285714285714286031 ),
 .UNSPECIFIED. ) 
 GEOMETRIC_REPRESENTATION_ITEM ( )  RATIONAL_B_SPLINE_SURFACE ( (
 ( 1.000000000000000000, 0.9510565162951535312, 1.000000000000000000, 0.9510565162951535312, 1.000000000000000000, 0.9510565162951535312, 1.000000000000000000, 0.9510565162951535312, 1.000000000000000000, 0.9510565162951535312, 1.000000000000000000, 0.9510565162951535312, 1.000000000000000000, 0.9510565162951535312, 1.000000000000000000, 0.9510565162951535312, 1.000000000000000000, 0.9510565162951535312, 1.000000000000000000, 0.9510565162951535312, 1.000000000000000000, 0.9510565162951535312, 1.000000000000000000, 0.9510565162951535312, 1.000000000000000000, 0.9510565162951535312, 1.000000000000000000, 0.9510565162951535312, 1.000000000000000000, 0.9510565162951535312, 1.000000000000000000, 0.9510565162951535312, 1.000000000000000000, 0.9510565162951535312, 1.000000000000000000, 0.9510565162951535312, 1.000000000000000000, 0.9510565162951535312, 1.000000000000000000, 0.9510565162951535312, 1.000000000000000000, 0.9510565162951535312, 1.000000000000000000, 0.9510565162951535312, 1.000000000000000000, 0.9510565162951535312, 1.000000000000000000, 0.9510565162951535312, 1.000000000000000000, 0.9510565162951535312, 1.000000000000000000, 0.9510565162951535312, 1.000000000000000000, 0.9510565162951535312, 1.000000000000000000, 0.9510565162951535312, 1.000000000000000000, 0.9510565162951535312, 1.000000000000000000, 0.9510565162951535312, 1.000000000000000000, 0.9510565162951535312, 1.000000000000000000, 0.9510565162951535312, 1.000000000000000000, 0.9510565162951535312, 1.000000000000000000, 0.9510565162951535312, 1.000000000000000000, 0.9510565162951535312, 1.000000000000000000, 0.9510565162951535312, 1.000000000000000000, 0.9510565162951535312, 1.000000000000000000, 0.9510565162951535312, 1.000000000000000000, 0.9510565162951535312, 1.000000000000000000, 0.9510565162951535312, 1.000000000000000000, 0.9510565162951535312, 1.000000000000000000, 0.9510565162951535312, 1.000000000000000000, 0.9510565162951535312, 1.000000000000000000, 0.9510565162951535312, 1.000000000000000000, 0.9510565162951535312, 1.000000000000000000, 0.9510565162951535312, 1.000000000000000000, 0.9510565162951535312, 1.000000000000000000, 0.9510565162951535312, 1.000000000000000000, 0.9510565162951535312, 1.000000000000000000, 0.9510565162951535312, 1.000000000000000000, 0.9510565162951535312, 1.000000000000000000, 0.9510565162951535312, 1.000000000000000000, 0.9510565162951535312, 1.000000000000000000, 0.9510565162951535312, 1.000000000000000000, 0.9510565162951535312, 1.000000000000000000, 0.9510565162951535312, 1.000000000000000000, 0.9510565162951535312, 1.000000000000000000, 0.9510565162951535312, 1.000000000000000000, 0.9510565162951535312, 1.000000000000000000, 0.9510565162951535312, 1.000000000000000000, 0.9510565162951535312, 1.000000000000000000, 0.9510565162951535312, 1.000000000000000000, 0.9510565162951535312, 1.000000000000000000, 0.9510565162951535312, 1.000000000000000000, 0.9510565162951535312, 1.000000000000000000),
 ( 0.3333333333333333703, 0.3170188387650512141, 0.3333333333333333703, 0.3170188387650512141, 0.3333333333333333703, 0.3170188387650512141, 0.3333333333333333703, 0.3170188387650512141, 0.3333333333333333703, 0.3170188387650512141, 0.3333333333333333703, 0.3170188387650512141, 0.3333333333333333703, 0.3170188387650512141, 0.3333333333333333703, 0.3170188387650512141, 0.3333333333333333703, 0.3170188387650512141, 0.3333333333333333703, 0.3170188387650512141, 0.3333333333333333703, 0.3170188387650512141, 0.3333333333333333703, 0.3170188387650512141, 0.3333333333333333703, 0.3170188387650512141, 0.3333333333333333703, 0.3170188387650512141, 0.3333333333333333703, 0.3170188387650512141, 0.3333333333333333703, 0.3170188387650512141, 0.3333333333333333703, 0.3170188387650512141, 0.3333333333333333703, 0.3170188387650512141, 0.3333333333333333703, 0.3170188387650512141, 0.3333333333333333703, 0.3170188387650512141, 0.3333333333333333703, 0.3170188387650512141, 0.3333333333333333703, 0.3170188387650512141, 0.3333333333333333703, 0.3170188387650512141, 0.3333333333333333703, 0.3170188387650512141, 0.3333333333333333703, 0.3170188387650512141, 0.3333333333333333703, 0.3170188387650512141, 0.3333333333333333703, 0.3170188387650512141, 0.3333333333333333703, 0.3170188387650512141, 0.3333333333333333703, 0.3170188387650512141, 0.3333333333333333703, 0.3170188387650512141, 0.3333333333333333703, 0.3170188387650512141, 0.3333333333333333703, 0.3170188387650512141, 0.3333333333333333703, 0.3170188387650512141, 0.3333333333333333703, 0.3170188387650512141, 0.3333333333333333703, 0.3170188387650512141, 0.3333333333333333703, 0.3170188387650512141, 0.3333333333333333703, 0.3170188387650512141, 0.3333333333333333703, 0.3170188387650512141, 0.3333333333333333703, 0.3170188387650512141, 0.3333333333333333703, 0.3170188387650512141, 0.3333333333333333703, 0.3170188387650512141, 0.3333333333333333703, 0.3170188387650512141, 0.3333333333333333703, 0.3170188387650512141, 0.3333333333333333703, 0.3170188387650512141, 0.3333333333333333703, 0.3170188387650512141, 0.3333333333333333703, 0.3170188387650512141, 0.3333333333333333703, 0.3170188387650512141, 0.3333333333333333703, 0.3170188387650512141, 0.3333333333333333703, 0.3170188387650512141, 0.3333333333333333703, 0.3170188387650512141, 0.3333333333333333703, 0.3170188387650512141, 0.3333333333333333703, 0.3170188387650512141, 0.3333333333333333703, 0.3170188387650512141, 0.3333333333333333703, 0.3170188387650512141, 0.3333333333333333703, 0.3170188387650512141, 0.3333333333333333703, 0.3170188387650512141, 0.3333333333333333703, 0.3170188387650512141, 0.3333333333333333703, 0.3170188387650512141, 0.3333333333333333703, 0.3170188387650512141, 0.3333333333333333703, 0.3170188387650512141, 0.3333333333333333703, 0.3170188387650512141, 0.3333333333333333703, 0.3170188387650512141, 0.3333333333333333703, 0.3170188387650512141, 0.3333333333333333703, 0.3170188387650512141, 0.3333333333333333703, 0.3170188387650512141, 0.3333333333333333703),
 ( 0.3333333333333333703, 0.3170188387650512141, 0.3333333333333333703, 0.3170188387650512141, 0.3333333333333333703, 0.3170188387650512141, 0.3333333333333333703, 0.3170188387650512141, 0.3333333333333333703, 0.3170188387650512141, 0.3333333333333333703, 0.3170188387650512141, 0.3333333333333333703, 0.3170188387650512141, 0.3333333333333333703, 0.3170188387650512141, 0.3333333333333333703, 0.3170188387650512141, 0.3333333333333333703, 0.3170188387650512141, 0.3333333333333333703, 0.3170188387650512141, 0.3333333333333333703, 0.3170188387650512141, 0.3333333333333333703, 0.3170188387650512141, 0.3333333333333333703, 0.3170188387650512141, 0.3333333333333333703, 0.3170188387650512141, 0.3333333333333333703, 0.3170188387650512141, 0.3333333333333333703, 0.3170188387650512141, 0.3333333333333333703, 0.3170188387650512141, 0.3333333333333333703, 0.3170188387650512141, 0.3333333333333333703, 0.3170188387650512141, 0.3333333333333333703, 0.3170188387650512141, 0.3333333333333333703, 0.3170188387650512141, 0.3333333333333333703, 0.3170188387650512141, 0.3333333333333333703, 0.3170188387650512141, 0.3333333333333333703, 0.3170188387650512141, 0.3333333333333333703, 0.3170188387650512141, 0.3333333333333333703, 0.3170188387650512141, 0.3333333333333333703, 0.3170188387650512141, 0.3333333333333333703, 0.3170188387650512141, 0.3333333333333333703, 0.3170188387650512141, 0.3333333333333333703, 0.3170188387650512141, 0.3333333333333333703, 0.3170188387650512141, 0.3333333333333333703, 0.3170188387650512141, 0.3333333333333333703, 0.3170188387650512141, 0.3333333333333333703, 0.3170188387650512141, 0.3333333333333333703, 0.3170188387650512141, 0.3333333333333333703, 0.3170188387650512141, 0.3333333333333333703, 0.3170188387650512141, 0.3333333333333333703, 0.3170188387650512141, 0.3333333333333333703, 0.3170188387650512141, 0.3333333333333333703, 0.3170188387650512141, 0.3333333333333333703, 0.3170188387650512141, 0.3333333333333333703, 0.3170188387650512141, 0.3333333333333333703, 0.3170188387650512141, 0.3333333333333333703, 0.3170188387650512141, 0.3333333333333333703, 0.3170188387650512141, 0.3333333333333333703, 0.3170188387650512141, 0.3333333333333333703, 0.3170188387650512141, 0.3333333333333333703, 0.3170188387650512141, 0.3333333333333333703, 0.3170188387650512141, 0.3333333333333333703, 0.3170188387650512141, 0.3333333333333333703, 0.3170188387650512141, 0.3333333333333333703, 0.3170188387650512141, 0.3333333333333333703, 0.3170188387650512141, 0.3333333333333333703, 0.3170188387650512141, 0.3333333333333333703, 0.3170188387650512141, 0.3333333333333333703, 0.3170188387650512141, 0.3333333333333333703, 0.3170188387650512141, 0.3333333333333333703, 0.3170188387650512141, 0.3333333333333333703, 0.3170188387650512141, 0.3333333333333333703, 0.3170188387650512141, 0.3333333333333333703, 0.3170188387650512141, 0.3333333333333333703, 0.3170188387650512141, 0.3333333333333333703, 0.3170188387650512141, 0.3333333333333333703, 0.3170188387650512141, 0.3333333333333333703),
 ( 1.000000000000000000, 0.9510565162951535312, 1.000000000000000000, 0.9510565162951535312, 1.000000000000000000, 0.9510565162951535312, 1.000000000000000000, 0.9510565162951535312, 1.000000000000000000, 0.9510565162951535312, 1.000000000000000000, 0.9510565162951535312, 1.000000000000000000, 0.9510565162951535312, 1.000000000000000000, 0.9510565162951535312, 1.000000000000000000, 0.9510565162951535312, 1.000000000000000000, 0.9510565162951535312, 1.000000000000000000, 0.9510565162951535312, 1.000000000000000000, 0.9510565162951535312, 1.000000000000000000, 0.9510565162951535312, 1.000000000000000000, 0.9510565162951535312, 1.000000000000000000, 0.9510565162951535312, 1.000000000000000000, 0.9510565162951535312, 1.000000000000000000, 0.9510565162951535312, 1.000000000000000000, 0.9510565162951535312, 1.000000000000000000, 0.9510565162951535312, 1.000000000000000000, 0.9510565162951535312, 1.000000000000000000, 0.9510565162951535312, 1.000000000000000000, 0.9510565162951535312, 1.000000000000000000, 0.9510565162951535312, 1.000000000000000000, 0.9510565162951535312, 1.000000000000000000, 0.9510565162951535312, 1.000000000000000000, 0.9510565162951535312, 1.000000000000000000, 0.9510565162951535312, 1.000000000000000000, 0.9510565162951535312, 1.000000000000000000, 0.9510565162951535312, 1.000000000000000000, 0.9510565162951535312, 1.000000000000000000, 0.9510565162951535312, 1.000000000000000000, 0.9510565162951535312, 1.000000000000000000, 0.9510565162951535312, 1.000000000000000000, 0.9510565162951535312, 1.000000000000000000, 0.9510565162951535312, 1.000000000000000000, 0.9510565162951535312, 1.000000000000000000, 0.9510565162951535312, 1.000000000000000000, 0.9510565162951535312, 1.000000000000000000, 0.9510565162951535312, 1.000000000000000000, 0.9510565162951535312, 1.000000000000000000, 0.9510565162951535312, 1.000000000000000000, 0.9510565162951535312, 1.000000000000000000, 0.9510565162951535312, 1.000000000000000000, 0.9510565162951535312, 1.000000000000000000, 0.9510565162951535312, 1.000000000000000000, 0.9510565162951535312, 1.000000000000000000, 0.9510565162951535312, 1.000000000000000000, 0.9510565162951535312, 1.000000000000000000, 0.9510565162951535312, 1.000000000000000000, 0.9510565162951535312, 1.000000000000000000, 0.9510565162951535312, 1.000000000000000000, 0.9510565162951535312, 1.000000000000000000, 0.9510565162951535312, 1.000000000000000000, 0.9510565162951535312, 1.000000000000000000, 0.9510565162951535312, 1.000000000000000000, 0.9510565162951535312, 1.000000000000000000, 0.9510565162951535312, 1.000000000000000000, 0.9510565162951535312, 1.000000000000000000, 0.9510565162951535312, 1.000000000000000000, 0.9510565162951535312, 1.000000000000000000, 0.9510565162951535312, 1.000000000000000000, 0.9510565162951535312, 1.000000000000000000, 0.9510565162951535312, 1.000000000000000000, 0.9510565162951535312, 1.000000000000000000, 0.9510565162951535312, 1.000000000000000000),
 ( 0.3333333333333333703, 0.3170188387650512141, 0.3333333333333333703, 0.3170188387650512141, 0.3333333333333333703, 0.3170188387650512141, 0.3333333333333333703, 0.3170188387650512141, 0.3333333333333333703, 0.3170188387650512141, 0.3333333333333333703, 0.3170188387650512141, 0.3333333333333333703, 0.3170188387650512141, 0.3333333333333333703, 0.3170188387650512141, 0.3333333333333333703, 0.3170188387650512141, 0.3333333333333333703, 0.3170188387650512141, 0.3333333333333333703, 0.3170188387650512141, 0.3333333333333333703, 0.3170188387650512141, 0.3333333333333333703, 0.3170188387650512141, 0.3333333333333333703, 0.3170188387650512141, 0.3333333333333333703, 0.3170188387650512141, 0.3333333333333333703, 0.3170188387650512141, 0.3333333333333333703, 0.3170188387650512141, 0.3333333333333333703, 0.3170188387650512141, 0.3333333333333333703, 0.3170188387650512141, 0.3333333333333333703, 0.3170188387650512141, 0.3333333333333333703, 0.3170188387650512141, 0.3333333333333333703, 0.3170188387650512141, 0.3333333333333333703, 0.3170188387650512141, 0.3333333333333333703, 0.3170188387650512141, 0.3333333333333333703, 0.3170188387650512141, 0.3333333333333333703, 0.3170188387650512141, 0.3333333333333333703, 0.3170188387650512141, 0.3333333333333333703, 0.3170188387650512141, 0.3333333333333333703, 0.3170188387650512141, 0.3333333333333333703, 0.3170188387650512141, 0.3333333333333333703, 0.3170188387650512141, 0.3333333333333333703, 0.3170188387650512141, 0.3333333333333333703, 0.3170188387650512141, 0.3333333333333333703, 0.3170188387650512141, 0.3333333333333333703, 0.3170188387650512141, 0.3333333333333333703, 0.3170188387650512141, 0.3333333333333333703, 0.3170188387650512141, 0.3333333333333333703, 0.3170188387650512141, 0.3333333333333333703, 0.3170188387650512141, 0.3333333333333333703, 0.3170188387650512141, 0.3333333333333333703, 0.3170188387650512141, 0.3333333333333333703, 0.3170188387650512141, 0.3333333333333333703, 0.3170188387650512141, 0.3333333333333333703, 0.3170188387650512141, 0.3333333333333333703, 0.3170188387650512141, 0.3333333333333333703, 0.3170188387650512141, 0.3333333333333333703, 0.3170188387650512141, 0.3333333333333333703, 0.3170188387650512141, 0.3333333333333333703, 0.3170188387650512141, 0.3333333333333333703, 0.3170188387650512141, 0.3333333333333333703, 0.3170188387650512141, 0.3333333333333333703, 0.3170188387650512141, 0.3333333333333333703, 0.3170188387650512141, 0.3333333333333333703, 0.3170188387650512141, 0.3333333333333333703, 0.3170188387650512141, 0.3333333333333333703, 0.3170188387650512141, 0.3333333333333333703, 0.3170188387650512141, 0.3333333333333333703, 0.3170188387650512141, 0.3333333333333333703, 0.3170188387650512141, 0.3333333333333333703, 0.3170188387650512141, 0.3333333333333333703, 0.3170188387650512141, 0.3333333333333333703, 0.3170188387650512141, 0.3333333333333333703, 0.3170188387650512141, 0.3333333333333333703, 0.3170188387650512141, 0.3333333333333333703, 0.3170188387650512141, 0.3333333333333333703),
 ( 0.3333333333333333703, 0.3170188387650512141, 0.3333333333333333703, 0.3170188387650512141, 0.3333333333333333703, 0.3170188387650512141, 0.3333333333333333703, 0.3170188387650512141, 0.3333333333333333703, 0.3170188387650512141, 0.3333333333333333703, 0.3170188387650512141, 0.3333333333333333703, 0.3170188387650512141, 0.3333333333333333703, 0.3170188387650512141, 0.3333333333333333703, 0.3170188387650512141, 0.3333333333333333703, 0.3170188387650512141, 0.3333333333333333703, 0.3170188387650512141, 0.3333333333333333703, 0.3170188387650512141, 0.3333333333333333703, 0.3170188387650512141, 0.3333333333333333703, 0.3170188387650512141, 0.3333333333333333703, 0.3170188387650512141, 0.3333333333333333703, 0.3170188387650512141, 0.3333333333333333703, 0.3170188387650512141, 0.3333333333333333703, 0.3170188387650512141, 0.3333333333333333703, 0.3170188387650512141, 0.3333333333333333703, 0.3170188387650512141, 0.3333333333333333703, 0.3170188387650512141, 0.3333333333333333703, 0.3170188387650512141, 0.3333333333333333703, 0.3170188387650512141, 0.3333333333333333703, 0.3170188387650512141, 0.3333333333333333703, 0.3170188387650512141, 0.3333333333333333703, 0.3170188387650512141, 0.3333333333333333703, 0.3170188387650512141, 0.3333333333333333703, 0.3170188387650512141, 0.3333333333333333703, 0.3170188387650512141, 0.3333333333333333703, 0.3170188387650512141, 0.3333333333333333703, 0.3170188387650512141, 0.3333333333333333703, 0.3170188387650512141, 0.3333333333333333703, 0.3170188387650512141, 0.3333333333333333703, 0.3170188387650512141, 0.3333333333333333703, 0.3170188387650512141, 0.3333333333333333703, 0.3170188387650512141, 0.3333333333333333703, 0.3170188387650512141, 0.3333333333333333703, 0.3170188387650512141, 0.3333333333333333703, 0.3170188387650512141, 0.3333333333333333703, 0.3170188387650512141, 0.3333333333333333703, 0.3170188387650512141, 0.3333333333333333703, 0.3170188387650512141, 0.3333333333333333703, 0.3170188387650512141, 0.3333333333333333703, 0.3170188387650512141, 0.3333333333333333703, 0.3170188387650512141, 0.3333333333333333703, 0.3170188387650512141, 0.3333333333333333703, 0.3170188387650512141, 0.3333333333333333703, 0.3170188387650512141, 0.3333333333333333703, 0.3170188387650512141, 0.3333333333333333703, 0.3170188387650512141, 0.3333333333333333703, 0.3170188387650512141, 0.3333333333333333703, 0.3170188387650512141, 0.3333333333333333703, 0.3170188387650512141, 0.3333333333333333703, 0.3170188387650512141, 0.3333333333333333703, 0.3170188387650512141, 0.3333333333333333703, 0.3170188387650512141, 0.3333333333333333703, 0.3170188387650512141, 0.3333333333333333703, 0.3170188387650512141, 0.3333333333333333703, 0.3170188387650512141, 0.3333333333333333703, 0.3170188387650512141, 0.3333333333333333703, 0.3170188387650512141, 0.3333333333333333703, 0.3170188387650512141, 0.3333333333333333703, 0.3170188387650512141, 0.3333333333333333703, 0.3170188387650512141, 0.3333333333333333703, 0.3170188387650512141, 0.3333333333333333703),
 ( 1.000000000000000000, 0.9510565162951535312, 1.000000000000000000, 0.9510565162951535312, 1.000000000000000000, 0.9510565162951535312, 1.000000000000000000, 0.9510565162951535312, 1.000000000000000000, 0.9510565162951535312, 1.000000000000000000, 0.9510565162951535312, 1.000000000000000000, 0.9510565162951535312, 1.000000000000000000, 0.9510565162951535312, 1.000000000000000000, 0.9510565162951535312, 1.000000000000000000, 0.9510565162951535312, 1.000000000000000000, 0.9510565162951535312, 1.000000000000000000, 0.9510565162951535312, 1.000000000000000000, 0.9510565162951535312, 1.000000000000000000, 0.9510565162951535312, 1.000000000000000000, 0.9510565162951535312, 1.000000000000000000, 0.9510565162951535312, 1.000000000000000000, 0.9510565162951535312, 1.000000000000000000, 0.9510565162951535312, 1.000000000000000000, 0.9510565162951535312, 1.000000000000000000, 0.9510565162951535312, 1.000000000000000000, 0.9510565162951535312, 1.000000000000000000, 0.9510565162951535312, 1.000000000000000000, 0.9510565162951535312, 1.000000000000000000, 0.9510565162951535312, 1.000000000000000000, 0.9510565162951535312, 1.000000000000000000, 0.9510565162951535312, 1.000000000000000000, 0.9510565162951535312, 1.000000000000000000, 0.9510565162951535312, 1.000000000000000000, 0.9510565162951535312, 1.000000000000000000, 0.9510565162951535312, 1.000000000000000000, 0.9510565162951535312, 1.000000000000000000, 0.9510565162951535312, 1.000000000000000000, 0.9510565162951535312, 1.000000000000000000, 0.9510565162951535312, 1.000000000000000000, 0.9510565162951535312, 1.000000000000000000, 0.9510565162951535312, 1.000000000000000000, 0.9510565162951535312, 1.000000000000000000, 0.9510565162951535312, 1.000000000000000000, 0.9510565162951535312, 1.000000000000000000, 0.9510565162951535312, 1.000000000000000000, 0.9510565162951535312, 1.000000000000000000, 0.9510565162951535312, 1.000000000000000000, 0.9510565162951535312, 1.000000000000000000, 0.9510565162951535312, 1.000000000000000000, 0.9510565162951535312, 1.000000000000000000, 0.9510565162951535312, 1.000000000000000000, 0.9510565162951535312, 1.000000000000000000, 0.9510565162951535312, 1.000000000000000000, 0.9510565162951535312, 1.000000000000000000, 0.9510565162951535312, 1.000000000000000000, 0.9510565162951535312, 1.000000000000000000, 0.9510565162951535312, 1.000000000000000000, 0.9510565162951535312, 1.000000000000000000, 0.9510565162951535312, 1.000000000000000000, 0.9510565162951535312, 1.000000000000000000, 0.9510565162951535312, 1.000000000000000000, 0.9510565162951535312, 1.000000000000000000, 0.9510565162951535312, 1.000000000000000000, 0.9510565162951535312, 1.000000000000000000, 0.9510565162951535312, 1.000000000000000000, 0.9510565162951535312, 1.000000000000000000, 0.9510565162951535312, 1.000000000000000000, 0.9510565162951535312, 1.000000000000000000, 0.9510565162951535312, 1.000000000000000000, 0.9510565162951535312, 1.000000000000000000) ) ) 
 REPRESENTATION_ITEM ( '' )  SURFACE ( )  );
#1123 = PRODUCT_DEFINITION_CONTEXT ( 'detailed design', #4679, 'design' ) ;
#1124 = CARTESIAN_POINT ( 'NONE',  ( 8.731428362939190890, -13.89598863503036164, 27.21428571428572241 ) ) ;
#1125 = CARTESIAN_POINT ( 'NONE',  ( -8.621071003556675549, 13.96533075980314642, 10.21832628391215358 ) ) ;
#1126 = CARTESIAN_POINT ( 'NONE',  ( -14.26974319298268767, 1.607813917172874918, 29.35714285714285765 ) ) ;
#1127 = CARTESIAN_POINT ( 'NONE',  ( 6.717514421272239744, -6.717514421272154479, 16.50000000000001421 ) ) ;
#1128 = CARTESIAN_POINT ( 'NONE',  ( 1.689666864740335894, -10.36326688006720786, 5.798862081921429379 ) ) ;
#1129 = ORIENTED_EDGE ( 'NONE', *, *, #9823, .F. ) ;
#1130 = CARTESIAN_POINT ( 'NONE',  ( 11.85413878919593422, 7.448449071214774619, 19.71428571428571175 ) ) ;
#1131 = EDGE_LOOP ( 'NONE', ( #4189, #4952 ) ) ;
#1132 = PRODUCT_DEFINITION_FORMATION_WITH_SPECIFIED_SOURCE ( 'ANY', '', #9151, .NOT_KNOWN. ) ;
#1133 = CARTESIAN_POINT ( 'NONE',  ( -13.54758718765249625, -8.512513224245459753, 34.71428571428571530 ) ) ;
#1134 = CARTESIAN_POINT ( 'NONE',  ( -1.967016585148659846, 16.29368510291087091, 44.63881657323071295 ) ) ;
#1135 = CARTESIAN_POINT ( 'NONE',  ( 7.424621202458790314, -7.424621202458697944, 4.500000000000003553 ) ) ;
#1136 = CARTESIAN_POINT ( 'NONE',  ( -7.639999817571786700, 12.15899005565156266, 12.21428571428571708 ) ) ;
#1137 = ORIENTED_EDGE ( 'NONE', *, *, #2286, .T. ) ;
#1138 = CARTESIAN_POINT ( 'NONE',  ( -12.22833218042443271, 7.529642458189139909, 25.78167371608785530 ) ) ;
#1139 = VERTEX_POINT ( 'NONE', #7937 ) ;
#1140 = CARTESIAN_POINT ( 'NONE',  ( 6.188763155949558836, 12.71101015088858510, 48.72999999999996135 ) ) ;
#1141 = CARTESIAN_POINT ( 'NONE',  ( 13.89774397934249706, 1.693770420379375308, 40.13881657323070584 ) ) ;
#1142 = CARTESIAN_POINT ( 'NONE',  ( -7.390897758835869524, 7.458344646081637386, 14.00113791807859620 ) ) ;
#1143 = CARTESIAN_POINT ( 'NONE',  ( 9.377220287599001836, 4.724406229267492208, 2.901137918078569466 ) ) ;
#1144 = FACE_BOUND ( 'NONE', #6677, .T. ) ;
#1145 = CARTESIAN_POINT ( 'NONE',  ( 9.809645194534072132, -9.989344678689256796, 13.00404056962644006 ) ) ;
#1146 = ADVANCED_FACE ( 'NONE', ( #3187 ), #8668, .F. ) ;
#1147 = CARTESIAN_POINT ( 'NONE',  ( -7.424621202458789426, 7.424621202458724589, 12.00000000000001066 ) ) ;
#1148 = CARTESIAN_POINT ( 'NONE',  ( 5.297344310588354865, 15.53355953199867301, 39.06738800180213644 ) ) ;
#1149 = CARTESIAN_POINT ( 'NONE',  ( -7.316011149999984475, 12.10800216009354813, 48.73000000000000398 ) ) ;
#1150 = CARTESIAN_POINT ( 'NONE',  ( -1.791431617652833763, -15.89939535829188877, 21.85714285714286120 ) ) ;
#1151 = CARTESIAN_POINT ( 'NONE',  ( 11.40355824106246985, -11.22385875690704538, 10.99595943037356882 ) ) ;
#1152 = CARTESIAN_POINT ( 'NONE',  ( -108.0000000000000284, 0.000000000000000000, 0.000000000000000000 ) ) ;
#1153 = CARTESIAN_POINT ( 'NONE',  ( 9.873755945037075321, 1.513077731353043243, 3.051137918078546285 ) ) ;
#1155 = PRESENTATION_LAYER_ASSIGNMENT (  '', '', ( #6422 ) ) ;
#1154 = CARTESIAN_POINT ( 'NONE',  ( -1.486127417882243895, 9.383039235653816590, 15.29999999999997939 ) ) ;
#1156 = CARTESIAN_POINT ( 'NONE',  ( -163.9215233434256618, 1.865203048549891163, 14.88378837804381583 ) ) ;
#1157 = CARTESIAN_POINT ( 'NONE',  ( -7.639999817571787588, 12.15899005565156266, 36.21428571428573662 ) ) ;
#1158 = CARTESIAN_POINT ( 'NONE',  ( 1.567502665446232957, 13.91197093850540156, 42.85714285714285410 ) ) ;
#1159 = ORIENTED_EDGE ( 'NONE', *, *, #2378, .F. ) ;
#1160 = CIRCLE ( 'NONE', #5118, 1.000000000000000888 ) ;
#1161 = CARTESIAN_POINT ( 'NONE',  ( 5.420364854932001819, 15.49051278174644430, 43.07142857142858361 ) ) ;
#1162 = LINE ( 'NONE', #7464, #7266 ) ;
#1163 = AXIS2_PLACEMENT_3D ( 'NONE', #9798, #7508, #3574 ) ;
#1164 = CARTESIAN_POINT ( 'NONE',  ( 11.31370849898482334, -11.31370849898469366, 15.00000000000000000 ) ) ;
#1165 = DIRECTION ( 'NONE',  ( -1.000000000000000000, -0.000000000000000000, -0.000000000000000000 ) ) ;
#1166 = CARTESIAN_POINT ( 'NONE',  ( 7.027753727702739539, 7.098671581784288698, 16.74886208192143755 ) ) ;
#1167 = CARTESIAN_POINT ( 'NONE',  ( -1.513077731352923339, -9.873755945037078874, 5.948862081921430622 ) ) ;
#1168 = CARTESIAN_POINT ( 'NONE',  ( -13.82664651025767100, 8.841785722321537477, 3.789754855340718542 ) ) ;
#1169 = CONICAL_SURFACE ( 'NONE', #687, 1.610000000000000098, 0.7853981633974658205 ) ;
#1170 = CARTESIAN_POINT ( 'NONE',  ( -8.731428362939189114, 13.89598863503036341, 30.21428571428572596 ) ) ;
#1171 = AXIS2_PLACEMENT_3D ( 'NONE', #4561, #7661, #9318 ) ;
#1172 =( LENGTH_UNIT ( ) NAMED_UNIT ( * ) SI_UNIT ( .MILLI., .METRE. ) );
#1173 = CARTESIAN_POINT ( 'NONE',  ( -1.707986654103994528, 16.32287076676380266, 4.646897712483579745 ) ) ;
#1174 = CARTESIAN_POINT ( 'NONE',  ( 10.15407889436379030, 10.15407889436390576, 25.50000000000000711 ) ) ;
#1175 = ADVANCED_FACE ( 'NONE', ( #2510 ), #3234, .T. ) ;
#1176 = CARTESIAN_POINT ( 'NONE',  ( 15.89939535829187278, 1.791431617653015174, 2.142857142857140573 ) ) ;
#1177 = CARTESIAN_POINT ( 'NONE',  ( -5.110041130070070992, -16.97680807127747826, 0.000000000000000000 ) ) ;
#1178 = VERTEX_POINT ( 'NONE', #4737 ) ;
#1179 = CARTESIAN_POINT ( 'NONE',  ( 14.26974319298268767, -1.607813917172876916, 20.35714285714286476 ) ) ;
#1180 = AXIS2_PLACEMENT_3D ( 'NONE', #4946, #297, #8301 ) ;
#1181 = CARTESIAN_POINT ( 'NONE',  ( -8.731428362939187338, 13.89598863503036164, 36.21428571428572951 ) ) ;
#1182 = CARTESIAN_POINT ( 'NONE',  ( -8.404922754268618235, -13.61519076058357491, 48.28167371608785174 ) ) ;
#1183 = CARTESIAN_POINT ( 'NONE',  ( 9.355568503977840678, 4.766900247265305701, 18.90000000000002700 ) ) ;
#1184 = CARTESIAN_POINT ( 'NONE',  ( -9.899494936611716867, 9.899494936611610285, 5.999999999999998224 ) ) ;
#1185 = EDGE_CURVE ( 'NONE', #9817, #3385, #9399, .T. ) ;
#1186 = CARTESIAN_POINT ( 'NONE',  ( 7.340858601237956194, 11.92174236212700045, 21.28167371608785530 ) ) ;
#1187 = ORIENTED_EDGE ( 'NONE', *, *, #8517, .F. ) ;
#1188 = CARTESIAN_POINT ( 'NONE',  ( -166.6500000000000341, 0.1077421301470921078, 13.00000000000000711 ) ) ;
#1189 = CARTESIAN_POINT ( 'NONE',  ( 8.442910196168311288, 4.355403765523574222, 4.898862081921403266 ) ) ;
#1190 = CARTESIAN_POINT ( 'NONE',  ( 14.26974319298268767, -1.607813917172876916, 2.357142857142856762 ) ) ;
#1191 = CARTESIAN_POINT ( 'NONE',  ( 9.355568503977840678, 4.766900247265305701, 3.899999999999959055 ) ) ;
#1192 = CARTESIAN_POINT ( 'NONE',  ( 1.595456901104624459, -10.37818827243064668, 0.8011379180785925813 ) ) ;
#1193 = CARTESIAN_POINT ( 'NONE',  ( -160.0000000000000284, -7.609196703745946707E-15, 0.000000000000000000 ) ) ;
#1194 = CARTESIAN_POINT ( 'NONE',  ( 10.24623928997352884, 10.06191849875416899, 35.50404056962644006 ) ) ;
#1195 = CARTESIAN_POINT ( 'NONE',  ( 1.693770420379222319, 13.89774397934251837, 28.86118342676929416 ) ) ;
#1196 = CARTESIAN_POINT ( 'NONE',  ( 1.642561882922480621, -10.37072757624891750, 7.800000000000029132 ) ) ;
#1197 = CARTESIAN_POINT ( 'NONE',  ( 16.32287076676382043, -1.707986654103810897, 34.35310228751642825 ) ) ;
#1198 = ORIENTED_EDGE ( 'NONE', *, *, #7313, .F. ) ;
#1199 = CARTESIAN_POINT ( 'NONE',  ( -2.956870951528623337, 13.71658267976582835, 48.73000000000004661 ) ) ;
#1200 = CARTESIAN_POINT ( 'NONE',  ( -5.284464991282755264, 15.10213328493384743, 24.42857142857143060 ) ) ;
#1201 = DIRECTION ( 'NONE',  ( -1.000000000000000000, 1.842239752758738928E-31, -1.780435181894459419E-32 ) ) ;
#1202 = CARTESIAN_POINT ( 'NONE',  ( 4.743843029824831525, -13.17239914596749095, 17.42453085894499409 ) ) ;
#1203 = CARTESIAN_POINT ( 'NONE',  ( -8.877401133907129704, 4.579542530753042406, 7.851137918078569200 ) ) ;
#1204 = CARTESIAN_POINT ( 'NONE',  ( 9.865911304835474738, 1.562606840307950051, 19.04999999999997939 ) ) ;
#1205 = CIRCLE ( 'NONE', #4016, 13.00000000000000533 ) ;
#1206 = DIRECTION ( 'NONE',  ( 1.000000000000000000, 0.000000000000000000, 0.000000000000000000 ) ) ;
#1207 = CARTESIAN_POINT ( 'NONE',  ( 11.85413878919593422, 7.448449071214774619, 25.71428571428571885 ) ) ;
#1208 = CARTESIAN_POINT ( 'NONE',  ( 1.607813917173038121, -14.26974319298267346, 33.64285714285715301 ) ) ;
#1209 = ORIENTED_EDGE ( 'NONE', *, *, #6503, .T. ) ;
#1210 = CARTESIAN_POINT ( 'NONE',  ( -15.89939535829186923, -1.791431617653016062, 41.14285714285714590 ) ) ;
#1211 = LINE ( 'NONE', #6933, #2321 ) ;
#1212 = CARTESIAN_POINT ( 'NONE',  ( 15.49051278174638036, 5.420364854932175014, 19.92857142857143771 ) ) ;
#1213 = LINE ( 'NONE', #6003, #3504 ) ;
#1214 = CYLINDRICAL_SURFACE ( 'NONE', #2628, 13.00000000000000178 ) ;
#1215 = PRODUCT_DEFINITION_SHAPE ( 'NONE', 'NONE',  #7252 ) ;
#1216 = CARTESIAN_POINT ( 'NONE',  ( -43.00000000000002842, 6.933347799794049071E-30, -9.629649721936179265E-31 ) ) ;
#1217 = CARTESIAN_POINT ( 'NONE',  ( -1.533232399700100057, 9.375578539472094519, 19.29886208192143471 ) ) ;
#1218 = CARTESIAN_POINT ( 'NONE',  ( -8.442910196168309511, -4.355403765523546689, 6.398862081921404155 ) ) ;
#1219 = UNCERTAINTY_MEASURE_WITH_UNIT (LENGTH_MEASURE( 1.000000000000000082E-05 ), #7838, 'distance_accuracy_value', 'NONE');
#1220 = CARTESIAN_POINT ( 'NONE',  ( 10.90442828429183919, 1.727091770866679532, 10.05000000000002736 ) ) ;
#1221 = CARTESIAN_POINT ( 'NONE',  ( 13.61519076058348254, 8.404922754268771001, 5.718326283912152697 ) ) ;
#1222 = CARTESIAN_POINT ( 'NONE',  ( -15.10213328493390961, 5.284464991282586510, 23.57142857142857650 ) ) ;
#1223 = SURFACE_STYLE_FILL_AREA ( #2208 ) ;
#1224 = AXIS2_PLACEMENT_3D ( 'NONE', #3055, #7082, #9483 ) ;
#1225 = CARTESIAN_POINT ( 'NONE',  ( 15.06016580658428694, -5.404401153735007846, 12.57546914105500768 ) ) ;
#1226 = CARTESIAN_POINT ( 'NONE',  ( -13.21436662431716869, 4.623906867372262752, 23.57142857142857650 ) ) ;
#1227 = CARTESIAN_POINT ( 'NONE',  ( -15.49051278174638036, -5.420364854932175902, 4.928571428571430602 ) ) ;
#1228 = CARTESIAN_POINT ( 'NONE',  ( -1.791431617652833763, -15.89939535829188877, 39.85714285714286120 ) ) ;
#1229 = ORIENTED_EDGE ( 'NONE', *, *, #3196, .T. ) ;
#1230 = CARTESIAN_POINT ( 'NONE',  ( 10.15407889436379030, 10.15407889436390576, 13.50000000000000178 ) ) ;
#1231 = CARTESIAN_POINT ( 'NONE',  ( -15.89939535829186923, -1.791431617653016062, 35.14285714285713880 ) ) ;
#1232 = CARTESIAN_POINT ( 'NONE',  ( 9.989344678689365153, -9.809645194533958446, 4.995959430373563492 ) ) ;
#1233 = CARTESIAN_POINT ( 'NONE',  ( -1.727091770866549414, -10.90442828429184630, 16.94999999999998863 ) ) ;
#1234 = CARTESIAN_POINT ( 'NONE',  ( 1.567502665446232957, 13.91197093850540156, 12.85714285714285943 ) ) ;
#1235 = ADVANCED_FACE ( 'NONE', ( #3964 ), #2048, .T. ) ;
#1236 = CARTESIAN_POINT ( 'NONE',  ( -14.28433602490915000, 1.478298951650542481, 25.35310228751642470 ) ) ;
#1237 = VERTEX_POINT ( 'NONE', #6418 ) ;
#1238 = CARTESIAN_POINT ( 'NONE',  ( -88.00000000000002842, 0.000000000000000000, 0.000000000000000000 ) ) ;
#1239 = CARTESIAN_POINT ( 'NONE',  ( -10.37818827243067688, 1.595456901104524761, 18.69886208192145816 ) ) ;
#1240 = CARTESIAN_POINT ( 'NONE',  ( -4.743843029824828861, 13.17239914596749450, 50.42453085894499765 ) ) ;
#1241 = CARTESIAN_POINT ( 'NONE',  ( 10.37072757624895836, -1.642561882922355609, 4.199999999999981526 ) ) ;
#1242 = CARTESIAN_POINT ( 'NONE',  ( -4.809394265263009061, -9.333916720356723928, 4.101137918078561206 ) ) ;
#1243 = PLANE ( 'NONE',  #8942 ) ;
#1244 = CARTESIAN_POINT ( 'NONE',  ( -12.08964793087886314, 7.750357176954159932, 27.78975485534072121 ) ) ;
#1245 = CARTESIAN_POINT ( 'NONE',  ( -7.806708723663830618, -7.806708723663901672, 5.250000000000008882 ) ) ;
#1246 = CARTESIAN_POINT ( 'NONE',  ( -5.404401153735176599, 15.06016580658422477, 44.42453085894499765 ) ) ;
#1247 = DIRECTION ( 'NONE',  ( 0.000000000000000000, 0.000000000000000000, 1.000000000000000000 ) ) ;
#1248 = CARTESIAN_POINT ( 'NONE',  ( -168.0000000000000284, -2.363368035607157783E-15, 0.000000000000000000 ) ) ;
#1249 = CARTESIAN_POINT ( 'NONE',  ( -1.441234910513241818, -13.92619789766829008, 11.85310228751642470 ) ) ;
#1250 = CARTESIAN_POINT ( 'NONE',  ( -9.873755945037078874, -1.513077731353019706, 13.55113791807856316 ) ) ;
#1251 = CARTESIAN_POINT ( 'NONE',  ( 4.534861676072320158, -8.900167166472098046, 16.64999999999999858 ) ) ;
#1252 = DIRECTION ( 'NONE',  ( -4.818676322157796389E-17, 1.000000000000000000, 0.000000000000000000 ) ) ;
#1253 = CARTESIAN_POINT ( 'NONE',  ( -9.809645194534070356, 9.989344678689256796, -1.995959430373561272 ) ) ;
#1254 = CARTESIAN_POINT ( 'NONE',  ( 13.55419868402807992, 4.742819248065648807, 37.92857142857143060 ) ) ;
#1255 = EDGE_LOOP ( 'NONE', ( #9651, #4833 ) ) ;
#1256 = CARTESIAN_POINT ( 'NONE',  ( 10.03895970123120307, 12.58845729673829972, 49.39149694378009769 ) ) ;
#1257 = CARTESIAN_POINT ( 'NONE',  ( -5.232950123192864567, 15.02148939460208332, -1.389475189636305469E-15 ) ) ;
#1258 = CARTESIAN_POINT ( 'NONE',  ( -1.791431617652833763, -15.89939535829188877, 27.85714285714285765 ) ) ;
#1259 = CYLINDRICAL_SURFACE ( 'NONE', #4163, 15.00000000000000000 ) ;
#1260 = SURFACE_STYLE_USAGE ( .BOTH. , #3745 ) ;
#1261 = B_SPLINE_CURVE_WITH_KNOTS ( 'NONE', 3,
 ( #8909, #4251, #3421, #4979, #3329, #8862, #1682, #6465, #3471, #2447, #325, #1775, #9539, #5592, #4825, #906, #4928, #4053, #7200, #8075, #6814, #5273, #2846, #2741, #3570, #4300 ),
 .UNSPECIFIED., .F., .F.,
 ( 4, 2, 2, 2, 2, 2, 2, 2, 2, 2, 2, 2, 4 ),
 ( 0.005163858345264566406, 0.005809185821787722637, 0.006454513298310878000, 0.006777177036572426191, 0.007099840774833974383, 0.007422504513095522574, 0.007745168251357070766, 0.008067831989618618957, 0.008390495727880167148, 0.008713159466141713605, 0.009035823204403263531, 0.009681150680926300933, 0.01032647815744933834 ),
 .UNSPECIFIED. ) ;
#1262 = CARTESIAN_POINT ( 'NONE',  ( -1.727091770866549414, -10.90442828429184630, 1.949999999999996181 ) ) ;
#1263 = CARTESIAN_POINT ( 'NONE',  ( 8.900167166472154889, -4.534861676072210024, 10.35000000000002274 ) ) ;
#1264 = CARTESIAN_POINT ( 'NONE',  ( 8.442910196168311288, 4.355403765523576887, 7.898862081921404155 ) ) ;
#1265 = CARTESIAN_POINT ( 'NONE',  ( 10.37072757624895836, -1.642561882922356498, 16.19999999999999218 ) ) ;
#1266 = CARTESIAN_POINT ( 'NONE',  ( 5.543385399275644332, 15.44746603149420494, 5.075469141055008571 ) ) ;
#1267 = CARTESIAN_POINT ( 'NONE',  ( 8.731428362939190890, -13.89598863503036164, 39.21428571428571530 ) ) ;
#1268 =( LENGTH_UNIT ( ) NAMED_UNIT ( * ) SI_UNIT ( .MILLI., .METRE. ) );
#1269 = CARTESIAN_POINT ( 'NONE',  ( 8.621071003556677326, -13.96533075980314287, 1.218326283912148922 ) ) ;
#1270 = CARTESIAN_POINT ( 'NONE',  ( -4.742819248065502258, -13.55419868402813677, 28.07142857142857295 ) ) ;
#1271 = CARTESIAN_POINT ( 'NONE',  ( -15.89939535829186923, -1.791431617653016062, 5.142857142857143238 ) ) ;
#1272 = CARTESIAN_POINT ( 'NONE',  ( -13.54758718765249625, -8.512513224245459753, 46.71428571428571530 ) ) ;
#1273 = ORIENTED_EDGE ( 'NONE', *, *, #3129, .T. ) ;
#1274 = EDGE_CURVE ( 'NONE', #4587, #9073, #27, .T. ) ;
#1275 = CARTESIAN_POINT ( 'NONE',  ( -9.355568503977838901, -4.766900247265279944, 17.39999999999997016 ) ) ;
#1276 = DIRECTION ( 'NONE',  ( 0.000000000000000000, 8.191099868251448390E-34, 1.000000000000000000 ) ) ;
#1277 = AXIS2_PLACEMENT_3D ( 'NONE', #1556, #518, #6800 ) ;
#1278 = CARTESIAN_POINT ( 'NONE',  ( 1.791431617652837316, 15.89939535829188877, 30.85714285714286120 ) ) ;
#1279 =( GEOMETRIC_REPRESENTATION_CONTEXT ( 3 ) GLOBAL_UNCERTAINTY_ASSIGNED_CONTEXT ( ( #2663 ) ) GLOBAL_UNIT_ASSIGNED_CONTEXT ( ( #102, #6345, #938 ) ) REPRESENTATION_CONTEXT ( 'NONE', 'WORKASPACE' ) );
#1280 = CARTESIAN_POINT ( 'NONE',  ( -4.619798703721853528, -13.59724543428036725, 6.067388001802139996 ) ) ;
#1281 = CARTESIAN_POINT ( 'NONE',  ( -9.355568503977838901, -4.766900247265280832, 14.39999999999996838 ) ) ;
#1282 = APPLICATION_PROTOCOL_DEFINITION ( 'draft international standard', 'automotive_design', 1998, #1512 ) ;
#1283 = CARTESIAN_POINT ( 'NONE',  ( 10.15407889436379030, 10.15407889436390221, 31.50000000000000711 ) ) ;
#1284 = CARTESIAN_POINT ( 'NONE',  ( -13.25633410266679313, 4.503970704919840529, 37.56738800180213644 ) ) ;
#1285 = PRESENTATION_LAYER_ASSIGNMENT (  '', '', ( #4095 ) ) ;
#1286 = ORIENTED_EDGE ( 'NONE', *, *, #4236, .T. ) ;
#1287 = CARTESIAN_POINT ( 'NONE',  ( 4.766900247265192903, 9.355568503977902850, 18.60000000000000497 ) ) ;
#1288 = CARTESIAN_POINT ( 'NONE',  ( -166.2435802567831331, 1.089887640161022464, 12.95446314200367155 ) ) ;
#1289 = CARTESIAN_POINT ( 'NONE',  ( -10.37818827243067688, 1.595456901104524761, 15.69886208192145816 ) ) ;
#1290 = CARTESIAN_POINT ( 'NONE',  ( 13.89774397934249706, 1.693770420379375308, 46.13881657323070584 ) ) ;
#1291 = CARTESIAN_POINT ( 'NONE',  ( -10.37072757624895836, 1.642561882922381145, 8.700000000000041922 ) ) ;
#1292 = CARTESIAN_POINT ( 'NONE',  ( 9.814260835641038128, -5.056896391392198709, 15.35113791807859229 ) ) ;
#1293 = FACE_OUTER_BOUND ( 'NONE', #9168, .T. ) ;
#1294 = LINE ( 'NONE', #4449, #2817 ) ;
#1295 = CARTESIAN_POINT ( 'NONE',  ( -9.809645194534070356, 9.989344678689256796, 28.00404056962643651 ) ) ;
#1296 = ADVANCED_FACE ( 'NONE', ( #760 ), #1735, .T. ) ;
#1297 = ORIENTED_EDGE ( 'NONE', *, *, #6791, .F. ) ;
#1298 = CARTESIAN_POINT ( 'NONE',  ( 1.727091770866550968, 10.90442828429187294, 9.449999999999988631 ) ) ;
#1299 = CARTESIAN_POINT ( 'NONE',  ( 8.404922754268618235, 13.61519076058357491, 33.28167371608784464 ) ) ;
#1300 = EDGE_CURVE ( 'NONE', #999, #2970, #2355, .T. ) ;
#1301 = CARTESIAN_POINT ( 'NONE',  ( -13.05196022747598050, 7.990434241189387166, 48.73000000000000398 ) ) ;
#1302 = CARTESIAN_POINT ( 'NONE',  ( -158.0000000000000284, -6.938893903907228378E-15, 0.000000000000000000 ) ) ;
#1303 = CARTESIAN_POINT ( 'NONE',  ( -7.340858601237953529, -11.92174236212700222, 18.28167371608785174 ) ) ;
#1304 = CARTESIAN_POINT ( 'NONE',  ( 9.375578539472099848, -1.533232399699986370, 18.20113791807854398 ) ) ;
#1305 = CARTESIAN_POINT ( 'NONE',  ( -8.877401133907129704, 4.579542530753042406, 4.851137918078532785 ) ) ;
#1306 = CARTESIAN_POINT ( 'NONE',  ( -163.0677270160816192, 0.9532360713981521405, 14.97024790547416373 ) ) ;
#1307 = CARTESIAN_POINT ( 'NONE',  ( 7.639999817571789364, -12.15899005565156266, 45.21428571428572951 ) ) ;
#1308 = CARTESIAN_POINT ( 'NONE',  ( 7.556039541191335474, 11.78653521626503320, -0.7102451446592792372 ) ) ;
#1309 = VERTEX_POINT ( 'NONE', #8613 ) ;
#1310 = CARTESIAN_POINT ( 'NONE',  ( 15.89939535829187278, 1.791431617653015174, 44.14285714285714590 ) ) ;
#1311 = EDGE_CURVE ( 'NONE', #9896, #7728, #8253, .T. ) ;
#1312 = CARTESIAN_POINT ( 'NONE',  ( -10.35053069349207178, 12.21555809740962495, 4.615094676506451939E-15 ) ) ;
#1313 = CARTESIAN_POINT ( 'NONE',  ( 11.31370849898482334, -11.31370849898469366, 27.00000000000000355 ) ) ;
#1314 = DIRECTION ( 'NONE',  ( -1.000000000000000000, 0.000000000000000000, 0.000000000000000000 ) ) ;
#1315 =( NAMED_UNIT ( * ) PLANE_ANGLE_UNIT ( ) SI_UNIT ( $, .RADIAN. ) );
#1316 = MECHANICAL_DESIGN_GEOMETRIC_PRESENTATION_REPRESENTATION (  '', ( #5298 ), #9743 ) ;
#1317 = DIRECTION ( 'NONE',  ( 0.000000000000000000, 0.000000000000000000, 1.000000000000000000 ) ) ;
#1318 = CARTESIAN_POINT ( 'NONE',  ( -1.562606840307830591, -9.865911304835476514, 7.950000000000040146 ) ) ;
#1319 = CARTESIAN_POINT ( 'NONE',  ( -8.442910196168309511, -4.355403765523544024, 3.398862081921444123 ) ) ;
#1320 = CARTESIAN_POINT ( 'NONE',  ( 4.766900247265192903, 9.355568503977902850, 12.59999999999999964 ) ) ;
#1321 = CARTESIAN_POINT ( 'NONE',  ( -1.791431617652833763, -15.89939535829188877, 45.85714285714286120 ) ) ;
#1322 = CARTESIAN_POINT ( 'NONE',  ( 1.707986654103998303, -16.32287076676380266, 25.64689771248357886 ) ) ;
#1323 = AXIS2_PLACEMENT_3D ( 'NONE', #6239, #7957, #5375 ) ;
#1324 = CARTESIAN_POINT ( 'NONE',  ( 11.85413878919593422, 7.448449071214774619, 19.71428571428571175 ) ) ;
#1325 = CARTESIAN_POINT ( 'NONE',  ( 16.30827793483735633, -1.837501619626142890, 2.357142857142856762 ) ) ;
#1326 = CARTESIAN_POINT ( 'NONE',  ( 13.54758718765249803, 8.512513224245457977, 43.71428571428572241 ) ) ;
#1327 = ORIENTED_EDGE ( 'NONE', *, *, #2410, .F. ) ;
#1328 = CARTESIAN_POINT ( 'NONE',  ( 5.012215536711511987, -9.837026868205999364, 16.64999999999999858 ) ) ;
#1329 = ORIENTED_EDGE ( 'NONE', *, *, #7762, .T. ) ;
#1330 = FACE_BOUND ( 'NONE', #2547, .T. ) ;
#1331 = CIRCLE ( 'NONE', #9599, 0.9906000000000003691 ) ;
#1332 = VECTOR ( 'NONE', #3264, 1000.000000000000000 ) ;
#1333 = AXIS2_PLACEMENT_3D ( 'NONE', #9076, #9227, #8341 ) ;
#1334 = CARTESIAN_POINT ( 'NONE',  ( -13.25633410266679313, 4.503970704919840529, 7.567388001802139108 ) ) ;
#1335 = CARTESIAN_POINT ( 'NONE',  ( 9.837026868206066865, -5.012215536711392083, 19.34999999999996945 ) ) ;
#1336 = CARTESIAN_POINT ( 'NONE',  ( -15.10213328493390961, 5.284464991282586510, 5.571428571428574728 ) ) ;
#1337 = CARTESIAN_POINT ( 'NONE',  ( 15.89939535829187278, 1.791431617653015174, 8.142857142857145902 ) ) ;
#1338 = APPLICATION_PROTOCOL_DEFINITION ( 'draft international standard', 'automotive_design', 1998, #4338 ) ;
#1339 = CARTESIAN_POINT ( 'NONE',  ( -13.91197093850538380, -1.567502665446387278, 29.14285714285714235 ) ) ;
#1340 = ADVANCED_FACE ( 'NONE', ( #3181 ), #7100, .F. ) ;
#1341 = AXIS2_PLACEMENT_3D ( 'NONE', #3965, #8237, #9078 ) ;
#1342 = TOROIDAL_SURFACE ( 'NONE', #9583, 3.299999999999999822, 0.2000000000000000111 ) ;
#1343 = EDGE_CURVE ( 'NONE', #8824, #4150, #5768, .T. ) ;
#1344 = CARTESIAN_POINT ( 'NONE',  ( -14.28433602490915000, 1.478298951650542481, 37.35310228751641404 ) ) ;
#1345 = ORIENTED_EDGE ( 'NONE', *, *, #5402, .F. ) ;
#1346 = FACE_OUTER_BOUND ( 'NONE', #2854, .T. ) ;
#1347 = CARTESIAN_POINT ( 'NONE',  ( 15.14410076328353227, -5.164528828830166063, 28.56738800180213644 ) ) ;
#1348 = CARTESIAN_POINT ( 'NONE',  ( 10.37818827243067510, -1.595456901104499225, 20.19886208192146526 ) ) ;
#1349 = CARTESIAN_POINT ( 'NONE',  ( 4.743843029824831525, -13.17239914596749095, 47.42453085894499765 ) ) ;
#1350 = CARTESIAN_POINT ( 'NONE',  ( 1.642561882922480621, -10.37072757624892638, 1.800000000000023803 ) ) ;
#1351 = CARTESIAN_POINT ( 'NONE',  ( -4.967534682030703586, 9.859792900771058299, 14.15113791807854327 ) ) ;
#1352 =( GEOMETRIC_REPRESENTATION_CONTEXT ( 3 ) GLOBAL_UNCERTAINTY_ASSIGNED_CONTEXT ( ( #4119 ) ) GLOBAL_UNIT_ASSIGNED_CONTEXT ( ( #8397, #9910, #4533 ) ) REPRESENTATION_CONTEXT ( 'NONE', 'WORKASPACE' ) );
#1353 = CARTESIAN_POINT ( 'NONE',  ( 4.200000000000009059, -1.802041971015319193E-33, -2.200000000000001066 ) ) ;
#1354 = CARTESIAN_POINT ( 'NONE',  ( -13.17239914596754424, 4.743843029824683200, 27.57546914105500946 ) ) ;
#1355 = CARTESIAN_POINT ( 'NONE',  ( -9.333916720356675967, -4.809394265263095214, 3.398862081921444123 ) ) ;
#1356 = CARTESIAN_POINT ( 'NONE',  ( 12.22833218042443271, -7.529642458189144349, 4.781673716087850856 ) ) ;
#1357 = CLOSED_SHELL ( 'NONE', ( #6188, #6338, #4207, #6354, #4057, #6193, #3933, #5342, #719 ) ) ;
#1358 = CARTESIAN_POINT ( 'NONE',  ( 7.806708723663832394, 7.806708723663930982, 6.749999999999960920 ) ) ;
#1359 = CIRCLE ( 'NONE', #1333, 3.632199999999998763 ) ;
#1360 = DIRECTION ( 'NONE',  ( -1.000000000000000000, -0.000000000000000000, -0.000000000000000000 ) ) ;
#1361 = CARTESIAN_POINT ( 'NONE',  ( 7.750357176954296712, -12.08964793087877787, 23.21024514465928235 ) ) ;
#1362 = CARTESIAN_POINT ( 'NONE',  ( 4.809394265263009061, 9.333916720356739916, -0.3988620819214416247 ) ) ;
#1363 = CARTESIAN_POINT ( 'NONE',  ( 4.490180821391514421, -8.922933199037139218, 3.651137918078570355 ) ) ;
#1364 = CARTESIAN_POINT ( 'NONE',  ( -164.8566404013504041, -2.149912913094245148, 12.82099350572476837 ) ) ;
#1365 = CARTESIAN_POINT ( 'NONE',  ( -1.607813917173034124, 14.26974319298267524, 42.64285714285715301 ) ) ;
#1366 = EDGE_CURVE ( 'NONE', #7651, #3104, #9591, .T. ) ;
#1367 = CARTESIAN_POINT ( 'NONE',  ( 9.809645194534072132, -9.989344678689256796, 1.004040569626440726 ) ) ;
#1368 = ORIENTED_EDGE ( 'NONE', *, *, #5122, .T. ) ;
#1369 = CARTESIAN_POINT ( 'NONE',  ( 8.841785722321695573, -13.82664651025757152, 5.210245144659280569 ) ) ;
#1370 = CARTESIAN_POINT ( 'NONE',  ( -88.00000000000002842, 0.000000000000000000, 0.000000000000000000 ) ) ;
#1371 = EDGE_CURVE ( 'NONE', #3156, #3923, #3906, .T. ) ;
#1372 = CARTESIAN_POINT ( 'NONE',  ( 1.837501619626330074, -16.30827793483733501, 33.64285714285715301 ) ) ;
#1373 = DIRECTION ( 'NONE',  ( -1.000000000000000000, 0.000000000000000000, 0.000000000000000000 ) ) ;
#1374 = AXIS2_PLACEMENT_3D ( 'NONE', #1059, #5794, #8174 ) ;
#1375 =( BOUNDED_CURVE ( )  B_SPLINE_CURVE ( 2, ( #9572, #5575, #8738, #7185, #7232, #101, #8849, #1658, #3254, #4860, #937, #5680, #9523, #8642, #1759, #4910, #1562, #986, #3361, #6496, #4708, #7857, #3557, #9775, #3510, #4386, #1860, #7537, #1184, #5058, #7486, #1090, #4334, #412, #5010, #260, #5824, #464, #5921, #4281, #5106, #3407, #6685, #2677, #7336, #7433, #309, #3603, #9047, #8204, #9870, #362, #9097, #5773, #4187, #2775, #8157, #1136, #6735, #6640, #1234, #1042, #2010, #8947, #9000, #2583, #1807, #6543, #4231, #9722, #5726, #6591, #7382, #3449, #8894, #5164, #2626, #1910, #9824, #2726, #5869, #1958, #8258, #8316, #4961, #8113, #2265, #7702, #2932, #6074, #9355, #5412, #4551, #8522, #10069, #4441, #1396, #7648, #2059, #621, #9973, #9202, #9305, #9250, #8412, #3870, #8471, #2985, #567, #3713, #2830, #3768, #2112, #5255, #2880, #7587, #2219, #6959, #1494, #1446, #6178, #4596, #6902, #6130, #10121, #5365, #6022, #5212, #7749, #8571, #670, #3823, #6797, #2170, #9152, #6849, #1339, #4647, #4493, #10019, #3038, #8362, #9925, #5313, #5974, #7801, #723, #1283, #513, #3659, #768, #4696, #1747, #1549, #4845, #2464, #9462, #10224, #2365, #87, #7169, #6279, #138, #6229, #3195, #5517, #7946, #874, #7121, #38, #9511, #5614, #2417, #3290, #6331, #3134, #3972, #4071, #9615, #5666, #5466, #8677, #1597, #3242, #6380, #7892, #4747, #923, #817, #5563, #9559, #8725, #1646, #4896, #6432, #4026, #2517, #8834, #4793, #7995, #8782, #1700, #7219, #8044, #973, #7013, #10171, #3085, #9405, #7843, #8628, #2316, #3916, #7061, #2760, #3348, #8097, #7322, #1025, #5909, #8144, #9034, #2614, #2713, #1945, #6529, #1794, #7370, #1998 ),
 .UNSPECIFIED., .F., .F. ) 
 B_SPLINE_CURVE_WITH_KNOTS ( ( 3, 2, 2, 2, 2, 2, 2, 2, 2, 2, 2, 2, 2, 2, 2, 2, 2, 2, 2, 2, 2, 2, 2, 2, 2, 2, 2, 2, 2, 2, 2, 2, 2, 2, 2, 2, 2, 2, 2, 2, 2, 2, 2, 2, 2, 2, 2, 2, 2, 2, 2, 2, 2, 2, 2, 2, 2, 2, 2, 2, 2, 2, 2, 2, 2, 2, 2, 2, 2, 2, 2, 2, 2, 2, 2, 2, 2, 2, 2, 2, 2, 2, 2, 2, 2, 2, 2, 2, 2, 2, 2, 2, 2, 2, 2, 2, 2, 2, 2, 2, 2, 2, 2, 2, 2, 2, 2, 2, 2, 2, 2, 2, 2, 2, 3 ),
 ( 0.000000000000000000, 0.007936507936507936067, 0.01587301587301587213, 0.02380952380952380820, 0.03174603174603174427, 0.03968253968253968034, 0.04761904761904761640, 0.05555555555555555247, 0.06349206349206348854, 0.07142857142857142461, 0.07936507936507936067, 0.08730158730158729674, 0.09523809523809523281, 0.1031746031746031689, 0.1111111111111111049, 0.1190476190476190410, 0.1269841269841269771, 0.1349206349206349131, 0.1428571428571428492, 0.1507936507936508130, 0.1587301587301587213, 0.1666666666666666574, 0.1746031746031745935, 0.1825396825396825295, 0.1904761904761904656, 0.1984126984126984017, 0.2063492063492063378, 0.2142857142857142738, 0.2222222222222222099, 0.2301587301587301460, 0.2380952380952380820, 0.2460317460317460181, 0.2539682539682539542, 0.2619047619047619180, 0.2698412698412698263, 0.2777777777777777901, 0.2857142857142856984, 0.2936507936507936622, 0.3015873015873016261, 0.3095238095238095344, 0.3174603174603174427, 0.3253968253968254065, 0.3333333333333333148, 0.3412698412698412787, 0.3492063492063491870, 0.3571428571428571508, 0.3650793650793650591, 0.3730158730158730229, 0.3809523809523809312, 0.3888888888888889506, 0.3968253968253968034, 0.4047619047619047117, 0.4126984126984126755, 0.4206349206349206393, 0.4285714285714285476, 0.4365079365079365115, 0.4444444444444444198, 0.4523809523809523836, 0.4603174603174602919, 0.4682539682539682557, 0.4761904761904761640, 0.4841269841269841279, 0.4920634920634920362, 0.5000000000000000000, 0.5079365079365079083, 0.5158730158730159276, 0.5238095238095238360, 0.5317460317460317443, 0.5396825396825396526, 0.5476190476190476719, 0.5555555555555555802, 0.5634920634920634885, 0.5714285714285713969, 0.5793650793650794162, 0.5873015873015873245, 0.5952380952380952328, 0.6031746031746032521, 0.6111111111111111605, 0.6190476190476190688, 0.6269841269841269771, 0.6349206349206348854, 0.6428571428571429047, 0.6507936507936508130, 0.6587301587301587213, 0.6666666666666666297, 0.6746031746031747600, 0.6825396825396825573, 0.6904761904761904656, 0.6984126984126983739, 0.7063492063492063933, 0.7142857142857143016, 0.7222222222222222099, 0.7301587301587301182, 0.7380952380952381375, 0.7460317460317460458, 0.7539682539682539542, 0.7619047619047618625, 0.7698412698412698818, 0.7777777777777779011, 0.7857142857142856984, 0.7936507936507936067, 0.8015873015873016261, 0.8095238095238094234, 0.8174603174603174427, 0.8253968253968253510, 0.8333333333333333703, 0.8412698412698412787, 0.8492063492063491870, 0.8571428571428570953, 0.8650793650793651146, 0.8730158730158730229, 0.8809523809523809312, 0.8888888888888888395, 0.8968253968253968589, 0.9023904529665215390 ),
 .UNSPECIFIED. ) 
 CURVE ( )  GEOMETRIC_REPRESENTATION_ITEM ( )  RATIONAL_B_SPLINE_CURVE ( ( 1.000000000000000000, 0.9749279121818236193, 1.000000000000000000, 0.9749279121818236193, 1.000000000000000000, 0.9749279121818236193, 1.000000000000000000, 0.9749279121818236193, 1.000000000000000000, 0.9749279121818236193, 1.000000000000000000, 0.9749279121818236193, 1.000000000000000000, 0.9749279121818236193, 1.000000000000000000, 0.9749279121818236193, 1.000000000000000000, 0.9749279121818236193, 1.000000000000000000, 0.9749279121818236193, 1.000000000000000000, 0.9749279121818236193, 1.000000000000000000, 0.9749279121818236193, 1.000000000000000000, 0.9749279121818236193, 1.000000000000000000, 0.9749279121818236193, 1.000000000000000000, 0.9749279121818236193, 1.000000000000000000, 0.9749279121818236193, 1.000000000000000000, 0.9749279121818236193, 1.000000000000000000, 0.9749279121818236193, 1.000000000000000000, 0.9749279121818236193, 1.000000000000000000, 0.9749279121818236193, 1.000000000000000000, 0.9749279121818236193, 1.000000000000000000, 0.9749279121818236193, 1.000000000000000000, 0.9749279121818236193, 1.000000000000000000, 0.9749279121818236193, 1.000000000000000000, 0.9749279121818236193, 1.000000000000000000, 0.9749279121818236193, 1.000000000000000000, 0.9749279121818236193, 1.000000000000000000, 0.9749279121818236193, 1.000000000000000000, 0.9749279121818236193, 1.000000000000000000, 0.9749279121818236193, 1.000000000000000000, 0.9749279121818236193, 1.000000000000000000, 0.9749279121818236193, 1.000000000000000000, 0.9749279121818236193, 1.000000000000000000, 0.9749279121818236193, 1.000000000000000000, 0.9749279121818236193, 1.000000000000000000, 0.9749279121818236193, 1.000000000000000000, 0.9749279121818236193, 1.000000000000000000, 0.9749279121818236193, 1.000000000000000000, 0.9749279121818236193, 1.000000000000000000, 0.9749279121818236193, 1.000000000000000000, 0.9749279121818236193, 1.000000000000000000, 0.9749279121818236193, 1.000000000000000000, 0.9749279121818236193, 1.000000000000000000, 0.9749279121818236193, 1.000000000000000000, 0.9749279121818236193, 1.000000000000000000, 0.9749279121818236193, 1.000000000000000000, 0.9749279121818236193, 1.000000000000000000, 0.9749279121818236193, 1.000000000000000000, 0.9749279121818236193, 1.000000000000000000, 0.9749279121818236193, 1.000000000000000000, 0.9749279121818236193, 1.000000000000000000, 0.9749279121818236193, 1.000000000000000000, 0.9749279121818236193, 1.000000000000000000, 0.9749279121818236193, 1.000000000000000000, 0.9749279121818236193, 1.000000000000000000, 0.9749279121818236193, 1.000000000000000000, 0.9749279121818236193, 1.000000000000000000, 0.9749279121818236193, 1.000000000000000000, 0.9749279121818236193, 1.000000000000000000, 0.9749279121818236193, 1.000000000000000000, 0.9749279121818236193, 1.000000000000000000, 0.9749279121818236193, 1.000000000000000000, 0.9749279121818236193, 1.000000000000000000, 0.9749279121818236193, 1.000000000000000000, 0.9749279121818236193, 1.000000000000000000, 0.9749279121818236193, 1.000000000000000000, 0.9749279121818236193, 1.000000000000000000, 0.9749279121818236193, 1.000000000000000000, 0.9749279121818236193, 1.000000000000000000, 0.9749279121818236193, 1.000000000000000000, 0.9749279121818236193, 1.000000000000000000, 0.9749279121818236193, 1.000000000000000000, 0.9749279121818236193, 1.000000000000000000, 0.9749279121818236193, 1.000000000000000000, 0.9749279121818236193, 1.000000000000000000, 0.9749279121818236193, 1.000000000000000000, 0.9749279121818236193, 1.000000000000000000, 0.9749279121818236193, 1.000000000000000000, 0.9749279121818236193, 1.000000000000000000, 0.9749279121818236193, 1.000000000000000000, 0.9749279121818236193, 1.000000000000000000, 0.9749279121818236193, 1.000000000000000000, 0.9749279121818236193, 1.000000000000000000, 0.9749279121818236193, 1.000000000000000000, 0.9749279121818236193, 1.000000000000000000, 0.9749279121818236193, 1.000000000000000000, 0.9749279121818236193, 1.000000000000000000, 0.9749279121818236193, 1.000000000000000000, 0.9749279121818236193, 1.000000000000000000, 0.9749279121818236193, 1.000000000000000000, 0.9749279121818236193, 1.000000000000000000, 0.9749279121818236193, 1.000000000000000000, 0.9749279121818236193, 1.000000000000000000, 0.9749279121818236193, 1.000000000000000000, 0.9749279121818236193, 1.000000000000000000, 0.9749279121818236193, 1.000000000000000000, 0.9749279121818236193, 1.000000000000000000, 0.9749279121818236193, 1.000000000000000000, 0.9749279121818236193, 1.000000000000000000, 0.9749279121818236193, 1.000000000000000000, 0.9749279121818236193, 1.000000000000000000, 0.9749279121818236193, 1.000000000000000000, 0.9749279121818236193, 1.000000000000000000, 0.9749279121818236193, 1.000000000000000000, 0.9749279121818236193, 1.000000000000000000, 0.9749279121818236193, 1.000000000000000000, 0.9749279121818236193, 1.000000000000000000, 0.9749279121818236193, 1.000000000000000000, 0.9749279121818236193, 1.000000000000000000, 0.9749279121818236193, 1.000000000000000000, 0.9749279121818236193, 1.000000000000000000, 0.9749279121818236193, 1.000000000000000000, 0.9749279121818236193, 1.000000000000000000, 0.9824195253882965773, 0.9894938054834332419 ) ) 
 REPRESENTATION_ITEM ( '' )  );
#1376 = CARTESIAN_POINT ( 'NONE',  ( 9.837026868206066865, -5.012215536711392083, 1.350000000000015188 ) ) ;
#1377 = CARTESIAN_POINT ( 'NONE',  ( 1.562606840307832368, 9.865911304835510265, 3.450000000000006839 ) ) ;
#1378 = CARTESIAN_POINT ( 'NONE',  ( 9.390499931835536884, -1.439022436064273158, 14.19886208192146171 ) ) ;
#1379 = DIRECTION ( 'NONE',  ( 0.000000000000000000, -6.338944243255235518E-49, 1.000000000000000000 ) ) ;
#1380 = CARTESIAN_POINT ( 'NONE',  ( 11.22385875690717683, -11.40355824106234373, 19.00404056962642940 ) ) ;
#1381 = CARTESIAN_POINT ( 'NONE',  ( 13.54758718765249803, 8.512513224245457977, 43.71428571428572241 ) ) ;
#1382 = CARTESIAN_POINT ( 'NONE',  ( 8.620103694221997515, 13.47998361472160767, 17.28975485534072121 ) ) ;
#1383 = CARTESIAN_POINT ( 'NONE',  ( 4.742819248065503146, 13.55419868402813677, 31.07142857142857295 ) ) ;
#1384 = CARTESIAN_POINT ( 'NONE',  ( -5.420364854931999155, -15.49051278174644253, 16.07142857142857650 ) ) ;
#1385 = CARTESIAN_POINT ( 'NONE',  ( -8.512513224245306986, -13.54758718765259218, 46.28571428571429180 ) ) ;
#1386 = ORIENTED_EDGE ( 'NONE', *, *, #2260, .F. ) ;
#1387 = CARTESIAN_POINT ( 'NONE',  ( -1.642561882922479732, 10.37072757624895303, 12.29999999999997762 ) ) ;
#1388 = FILL_AREA_STYLE ('',( #8463 ) ) ;
#1389 = CARTESIAN_POINT ( 'NONE',  ( 5.284464991282756152, -15.10213328493384743, 45.42857142857143060 ) ) ;
#1390 = DIRECTION ( 'NONE',  ( 1.000000000000000000, 0.000000000000000000, 0.000000000000000000 ) ) ;
#1391 = CARTESIAN_POINT ( 'NONE',  ( -1.737328882695368115, 14.25515036105620581, 8.638816573230704066 ) ) ;
#1392 = CARTESIAN_POINT ( 'NONE',  ( 7.458344646081711105, -7.390897758835786036, 2.498862081921459755 ) ) ;
#1393 = CARTESIAN_POINT ( 'NONE',  ( -11.31370849898482156, 11.31370849898469544, 0.000000000000000000 ) ) ;
#1394 = CARTESIAN_POINT ( 'NONE',  ( 16.30827793483735633, -1.837501619626142890, 2.357142857142856762 ) ) ;
#1395 = SHAPE_DEFINITION_REPRESENTATION ( #8314, #58 ) ;
#1396 = CARTESIAN_POINT ( 'NONE',  ( 13.21436662431716869, -4.623906867372263640, 20.57142857142857295 ) ) ;
#1397 = EDGE_LOOP ( 'NONE', ( #7018, #1159 ) ) ;
#1398 = CARTESIAN_POINT ( 'NONE',  ( 9.989344678689365153, -9.809645194533958446, 46.99595943037356705 ) ) ;
#1399 = VECTOR ( 'NONE', #8490, 1000.000000000000000 ) ;
#1400 = EDGE_LOOP ( 'NONE', ( #5003, #9129, #5622, #9488 ) ) ;
#1401 = CARTESIAN_POINT ( 'NONE',  ( 0.000000000000000000, -0.8865213383406622683, -1.535500000000078469 ) ) ;
#1402 = CARTESIAN_POINT ( 'NONE',  ( -1.665163862719845067, -15.91362231745477374, 17.85310228751642114 ) ) ;
#1403 = CARTESIAN_POINT ( 'NONE',  ( -5.284464991282755264, 15.10213328493384743, 0.4285714285714309346 ) ) ;
#1404 = CARTESIAN_POINT ( 'NONE',  ( 7.027753727702739539, 7.098671581784288698, 7.748862081921418010 ) ) ;
#1405 = CARTESIAN_POINT ( 'NONE',  ( 9.989344678689365153, -9.809645194533958446, 46.99595943037356705 ) ) ;
#1406 = CARTESIAN_POINT ( 'NONE',  ( -10.37072757624895836, 1.642561882922381145, 5.700000000000038369 ) ) ;
#1407 = CARTESIAN_POINT ( 'NONE',  ( 4.967534682030706250, -9.859792900771036983, 9.651137918078598332 ) ) ;
#1408 = CARTESIAN_POINT ( 'NONE',  ( -88.00000000000002842, 0.000000000000000000, 8.000000000000000000 ) ) ;
#1409 = CARTESIAN_POINT ( 'NONE',  ( -7.529642458189277576, 12.22833218042435455, 28.21832628391215181 ) ) ;
#1410 = SURFACE_SIDE_STYLE ('',( #7076 ) ) ;
#1411 = CARTESIAN_POINT ( 'NONE',  ( -1.441234910513241818, -13.92619789766829008, 5.853102287516418478 ) ) ;
#1412 = B_SPLINE_CURVE_WITH_KNOTS ( 'NONE', 3,
 ( #2256, #5357, #8715, #3863, #80, #9297, #2408, #7003, #762, #6949, #2211, #7055, #6170, #6122, #10216, #6321 ),
 .UNSPECIFIED., .F., .F.,
 ( 4, 2, 2, 2, 2, 2, 2, 4 ),
 ( 0.04369022279437502487, 0.04534324305125501248, 0.04699626330813499314, 0.05030230382189496835, 0.05195532407877494901, 0.05360834433565493662, 0.05526136459253491728, 0.05691438484941489795 ),
 .UNSPECIFIED. ) ;
#1413 = CARTESIAN_POINT ( 'NONE',  ( -9.355568503977838901, -4.766900247265280832, 2.400000000000013234 ) ) ;
#1414 = EDGE_CURVE ( 'NONE', #7327, #8995, #6320, .T. ) ;
#1415 = CARTESIAN_POINT ( 'NONE',  ( 11.31370849898482334, -11.31370849898469366, 27.00000000000000355 ) ) ;
#1416 = DIRECTION ( 'NONE',  ( -1.000000000000000000, -0.000000000000000000, -0.000000000000000000 ) ) ;
#1417 = CARTESIAN_POINT ( 'NONE',  ( 10.06191849875406064, 10.24623928997363187, 15.49595943037356882 ) ) ;
#1418 = CARTESIAN_POINT ( 'NONE',  ( -1.439022436064386845, 9.390499931835526226, 11.30113791807855961 ) ) ;
#1419 = CARTESIAN_POINT ( 'NONE',  ( 9.375578539472099848, -1.533232399699986370, 6.201137918078538647 ) ) ;
#1420 = DIRECTION ( 'NONE',  ( 0.000000000000000000, -1.000000000000000000, 0.000000000000000000 ) ) ;
#1421 = CARTESIAN_POINT ( 'NONE',  ( 10.15407889436379030, 10.15407889436390576, 43.50000000000000711 ) ) ;
#1422 = CARTESIAN_POINT ( 'NONE',  ( -4.865839792409144771, -13.51115193377589740, 2.075469141055009015 ) ) ;
#1423 = EDGE_LOOP ( 'NONE', ( #9348, #2777, #5681, #2103 ) ) ;
#1424 = CARTESIAN_POINT ( 'NONE',  ( -5.297344310588352201, -15.53355953199867301, 12.06738800180214000 ) ) ;
#1425 = DIRECTION ( 'NONE',  ( 0.000000000000000000, 0.000000000000000000, 1.000000000000000000 ) ) ;
#1426 = CARTESIAN_POINT ( 'NONE',  ( 1.837501619626330074, -16.30827793483733501, 27.64285714285714590 ) ) ;
#1427 = PLANE ( 'NONE',  #6944 ) ;
#1428 = CARTESIAN_POINT ( 'NONE',  ( -6.717514421272238856, 6.717514421272181124, 2.585396704745767526E-18 ) ) ;
#1429 = CARTESIAN_POINT ( 'NONE',  ( -6.717514421272238856, 6.717514421272181124, 12.00000000000001066 ) ) ;
#1430 = CARTESIAN_POINT ( 'NONE',  ( -9.858066664633883036, -1.612135949262831547, 18.54886208192142405 ) ) ;
#1431 = DIRECTION ( 'NONE',  ( -4.755747939841215952E-17, 1.000000000000000000, 0.000000000000000000 ) ) ;
#1432 = CARTESIAN_POINT ( 'NONE',  ( -5.420364854931999155, -15.49051278174644253, 46.07142857142856940 ) ) ;
#1433 =( LENGTH_UNIT ( ) NAMED_UNIT ( * ) SI_UNIT ( .MILLI., .METRE. ) );
#1434 = CARTESIAN_POINT ( 'NONE',  ( 15.53355953199861794, 5.297344310588528060, 23.93261199819786711 ) ) ;
#1435 = CARTESIAN_POINT ( 'NONE',  ( -17.72919999999999874, 2.171200803144325526E-15, -1.270000000000007123 ) ) ;
#1436 = VERTEX_POINT ( 'NONE', #7998 ) ;
#1437 = CARTESIAN_POINT ( 'NONE',  ( 5.012215536711511987, -9.837026868205999364, 10.65000000000000924 ) ) ;
#1438 = EDGE_LOOP ( 'NONE', ( #8309, #6120, #4912 ) ) ;
#1439 = CARTESIAN_POINT ( 'NONE',  ( 15.10213328493390783, -5.284464991282587398, 44.57142857142857650 ) ) ;
#1440 =( NAMED_UNIT ( * ) SI_UNIT ( $, .STERADIAN. ) SOLID_ANGLE_UNIT ( ) );
#1441 = COLOUR_RGB ( '', 0.08235294, 0.09019608, 0.10196078) ;
#1442 = CARTESIAN_POINT ( 'NONE',  ( -10.37818827243067688, 1.595456901104523428, 12.69886208192145816 ) ) ;
#1443 = CARTESIAN_POINT ( 'NONE',  ( 1.837501619626330074, -16.30827793483733501, 3.642857142857144126 ) ) ;
#1444 = CARTESIAN_POINT ( 'NONE',  ( -1.917699372585823570, -15.88516839912900558, 43.86118342676930126 ) ) ;
#1445 = CONTEXT_DEPENDENT_SHAPE_REPRESENTATION ( #1712, #8982 ) ;
#1446 = CARTESIAN_POINT ( 'NONE',  ( 10.15407889436379030, 10.15407889436390221, 25.50000000000000355 ) ) ;
#1447 = CARTESIAN_POINT ( 'NONE',  ( 4.503970704919991519, -13.25633410266674517, 31.43261199819787421 ) ) ;
#1448 = CARTESIAN_POINT ( 'NONE',  ( -8.900167166472160218, 4.534861676072235781, 5.849999999999989875 ) ) ;
#1449 = VECTOR ( 'NONE', #9977, 999.9999999999998863 ) ;
#1450 = CARTESIAN_POINT ( 'NONE',  ( 9.989344678689365153, -9.809645194533958446, 40.99595943037355994 ) ) ;
#1451 = ORIENTED_EDGE ( 'NONE', *, *, #7973, .T. ) ;
#1452 = CARTESIAN_POINT ( 'NONE',  ( -55.00000000000002132, 18.00000000000001776, -1.819825643106760428E-16 ) ) ;
#1453 = CARTESIAN_POINT ( 'NONE',  ( 11.40355824106246985, -11.22385875690704538, 22.99595943037356705 ) ) ;
#1454 = DIRECTION ( 'NONE',  ( 0.000000000000000000, -6.338944243255235518E-49, 1.000000000000000000 ) ) ;
#1455 = PRODUCT_RELATED_PRODUCT_CATEGORY ( 'part', '', ( #308 ) ) ;
#1456 = CARTESIAN_POINT ( 'NONE',  ( -1.665163862719845067, -15.91362231745477374, 23.85310228751642825 ) ) ;
#1457 = CARTESIAN_POINT ( 'NONE',  ( -108.0000000000000284, 15.99999999999999645, 0.000000000000000000 ) ) ;
#1458 = CARTESIAN_POINT ( 'NONE',  ( -4.809394265263009061, -9.333916720356718599, 10.10113791807856742 ) ) ;
#1459 = CARTESIAN_POINT ( 'NONE',  ( 2.000000000000001776, -1.773042676681352292, -1.110223024625156540E-13 ) ) ;
#1460 = CARTESIAN_POINT ( 'NONE',  ( -14.25515036105622890, 1.737328882695209575, 45.36118342676930837 ) ) ;
#1461 =( GEOMETRIC_REPRESENTATION_CONTEXT ( 3 ) GLOBAL_UNCERTAINTY_ASSIGNED_CONTEXT ( ( #1219 ) ) GLOBAL_UNIT_ASSIGNED_CONTEXT ( ( #7838, #3130, #5308 ) ) REPRESENTATION_CONTEXT ( 'NONE', 'WORKASPACE' ) );
#1462 = CARTESIAN_POINT ( 'NONE',  ( -9.989344678689363377, 9.809645194533960222, 1.995959430373561272 ) ) ;
#1463 = CARTESIAN_POINT ( 'NONE',  ( -7.424621202458789426, 7.424621202458724589, 6.000000000000005329 ) ) ;
#1464 = CARTESIAN_POINT ( 'NONE',  ( -4.169902070941136074, -13.58603705635637482, -1.270000000000007123 ) ) ;
#1465 = CARTESIAN_POINT ( 'NONE',  ( 4.743843029824831525, -13.17239914596749095, 29.42453085894499765 ) ) ;
#1466 = CARTESIAN_POINT ( 'NONE',  ( 7.098671581784200768, 7.027753727702831021, 11.75113791807857666 ) ) ;
#1467 = CARTESIAN_POINT ( 'NONE',  ( 1.612135949262739398, 9.858066664633913234, 5.451137918078557298 ) ) ;
#1468 = CARTESIAN_POINT ( 'NONE',  ( -165.1407354622004391, -2.150086286197278707, 12.82096443211790060 ) ) ;
#1469 = CARTESIAN_POINT ( 'NONE',  ( -5.164528828830334817, 15.14410076328347543, 40.43261199819787066 ) ) ;
#1470 = CARTESIAN_POINT ( 'NONE',  ( 1.607813917173038121, -14.26974319298267346, 39.64285714285716722 ) ) ;
#1471 = CARTESIAN_POINT ( 'NONE',  ( -1.478298951650703019, 14.28433602490913579, 4.646897712483579745 ) ) ;
#1472 = ORIENTED_EDGE ( 'NONE', *, *, #9157, .F. ) ;
#1473 = EDGE_CURVE ( 'NONE', #6295, #7986, #3303, .T. ) ;
#1474 = CARTESIAN_POINT ( 'NONE',  ( -15.14410076328353227, 5.164528828830164287, 13.56738800180213822 ) ) ;
#1475 = PLANE ( 'NONE',  #8773 ) ;
#1476 = ADVANCED_FACE ( 'NONE', ( #9765 ), #1082, .T. ) ;
#1477 = CARTESIAN_POINT ( 'NONE',  ( 15.10213328493390783, -5.284464991282587398, 38.57142857142857650 ) ) ;
#1478 = DIRECTION ( 'NONE',  ( 1.000000000000000000, 0.000000000000000000, 0.000000000000000000 ) ) ;
#1479 = CARTESIAN_POINT ( 'NONE',  ( -68.00000000000002842, 0.000000000000000000, 0.000000000000000000 ) ) ;
#1480 = CARTESIAN_POINT ( 'NONE',  ( -6.717514421272238856, 6.717514421272180236, 9.000000000000007105 ) ) ;
#1481 = CARTESIAN_POINT ( 'NONE',  ( 6.751237864895159646, -6.683790977649239906, 20.49886208192143400 ) ) ;
#1482 = CARTESIAN_POINT ( 'NONE',  ( 56.99999999999997158, 0.000000000000000000, 6.999999999999999112 ) ) ;
#1483 = CARTESIAN_POINT ( 'NONE',  ( -15.89939535829186923, -1.791431617653016062, 41.14285714285714590 ) ) ;
#1484 = CARTESIAN_POINT ( 'NONE',  ( -16.29368510291090288, 1.967016585148476215, 15.36118342676929771 ) ) ;
#1485 = CARTESIAN_POINT ( 'NONE',  ( 15.49051278174638036, 5.420364854932175014, 19.92857142857143771 ) ) ;
#1486 = CARTESIAN_POINT ( 'NONE',  ( 57.99999999999997158, 0.000000000000000000, 8.000000000000000000 ) ) ;
#1487 = CARTESIAN_POINT ( 'NONE',  ( -10.90442828429183919, -1.727091770866654663, 11.54999999999998295 ) ) ;
#1488 = CARTESIAN_POINT ( 'NONE',  ( -16.30827793483735988, 1.837501619626141558, 47.35714285714286120 ) ) ;
#1489 = SHAPE_REPRESENTATION_RELATIONSHIP ( 'NONE' , 'NONE' ,  #8171, #67 ) ;
#1490 = CARTESIAN_POINT ( 'NONE',  ( -7.458344646081709328, 7.390897758835805575, 6.998862081921422451 ) ) ;
#1491 = CIRCLE ( 'NONE', #7429, 1.610000000000000098 ) ;
#1492 = CARTESIAN_POINT ( 'NONE',  ( 5.164528828830335705, -15.14410076328347543, 43.43261199819787066 ) ) ;
#1493 = ITEM_DEFINED_TRANSFORMATION ( 'NONE', 'NONE', #2114,  #3995 ) ;
#1494 = CARTESIAN_POINT ( 'NONE',  ( 7.448449071214646722, 11.85413878919601594, 25.28571428571428470 ) ) ;
#1495 = ADVANCED_FACE ( 'NONE', ( #5050 ), #926, .T. ) ;
#1496 = CARTESIAN_POINT ( 'NONE',  ( 8.464561979789474222, 4.312909747525755400, 12.90000000000002345 ) ) ;
#1497 = ORIENTED_EDGE ( 'NONE', *, *, #1343, .F. ) ;
#1498 = CARTESIAN_POINT ( 'NONE',  ( -7.750357176954294935, 12.08964793087877787, 38.21024514465928235 ) ) ;
#1499 = VERTEX_POINT ( 'NONE', #2520 ) ;
#1500 = CARTESIAN_POINT ( 'NONE',  ( -108.0000000000000284, 0.000000000000000000, 15.99999999999999645 ) ) ;
#1501 = CARTESIAN_POINT ( 'NONE',  ( -1.967016585148659846, 16.29368510291087091, 26.63881657323070939 ) ) ;
#1502 = CARTESIAN_POINT ( 'NONE',  ( 13.89598863503045933, -8.731428362939032795, 2.785714285714283367 ) ) ;
#1503 = CARTESIAN_POINT ( 'NONE',  ( 5.404401153735178376, -15.06016580658422477, 17.42453085894499409 ) ) ;
#1504 = CARTESIAN_POINT ( 'NONE',  ( 13.61000000000001720, 2.449293598294708386E-16, -2.000000000000001332 ) ) ;
#1505 = CARTESIAN_POINT ( 'NONE',  ( -9.814260835641038128, 5.056896391392218248, 16.85113791807854611 ) ) ;
#1506 = DIRECTION ( 'NONE',  ( -6.162975822039154730E-33, -0.4999999999999991118, 0.8660254037844391517 ) ) ;
#1507 = AXIS2_PLACEMENT_3D ( 'NONE', #10054, #8611, #3805 ) ;
#1508 = EDGE_CURVE ( 'NONE', #3127, #9396, #1750, .T. ) ;
#1509 = CIRCLE ( 'NONE', #9927, 2.000000000000000888 ) ;
#1510 = ADVANCED_FACE ( 'NONE', ( #9562 ), #7923, .T. ) ;
#1511 = CARTESIAN_POINT ( 'NONE',  ( -1.737328882695368115, 14.25515036105620581, 8.638816573230704066 ) ) ;
#1512 = APPLICATION_CONTEXT ( 'automotive_design' ) ;
#1513 = ORIENTED_EDGE ( 'NONE', *, *, #7634, .T. ) ;
#1514 = CARTESIAN_POINT ( 'NONE',  ( -7.424621202458789426, 7.424621202458724589, -3.058133128536869244E-17 ) ) ;
#1515 = CARTESIAN_POINT ( 'NONE',  ( 13.54758718765249803, 8.512513224245457977, 31.71428571428571530 ) ) ;
#1516 = DIRECTION ( 'NONE',  ( 0.000000000000000000, 6.938893903907221444E-18, 1.000000000000000000 ) ) ;
#1517 = COLOUR_RGB ( '', 0.40784314, 0.44705882, 0.49803922) ;
#1518 = CARTESIAN_POINT ( 'NONE',  ( 7.340858601237956194, 11.92174236212700045, 27.28167371608785174 ) ) ;
#1519 = CARTESIAN_POINT ( 'NONE',  ( -4.967534682030703586, 9.859792900771061852, 2.151137918078574796 ) ) ;
#1520 = CARTESIAN_POINT ( 'NONE',  ( -9.375578539472099848, 1.533232399700011461, 1.701137918078535094 ) ) ;
#1521 = CARTESIAN_POINT ( 'NONE',  ( -163.0673332015201709, -0.9523206289711777517, 12.96571997834879397 ) ) ;
#1522 = CARTESIAN_POINT ( 'NONE',  ( 5.543385399275644332, 15.44746603149420494, 47.07546914105501656 ) ) ;
#1523 = CARTESIAN_POINT ( 'NONE',  ( 10.24623928997352884, 10.06191849875416899, 5.504040569626439172 ) ) ;
#1524 = CARTESIAN_POINT ( 'NONE',  ( -12.08964793087886314, 7.750357176954159932, 3.789754855340718542 ) ) ;
#1525 = ORIENTED_EDGE ( 'NONE', *, *, #716, .T. ) ;
#1526 = AXIS2_PLACEMENT_3D ( 'NONE', #4077, #8682, #4034 ) ;
#1527 = CARTESIAN_POINT ( 'NONE',  ( -5.110041130070070992, -16.97680807127747826, -1.270000000000007123 ) ) ;
#1528 = CARTESIAN_POINT ( 'NONE',  ( -8.512513224245306986, -13.54758718765259218, 40.28571428571428470 ) ) ;
#1529 = DIRECTION ( 'NONE',  ( -1.000000000000000000, 0.000000000000000000, -0.000000000000000000 ) ) ;
#1530 = PLANE ( 'NONE',  #826 ) ;
#1531 = CARTESIAN_POINT ( 'NONE',  ( -4.534861676072319270, 8.900167166472121139, 12.14999999999996305 ) ) ;
#1532 = CARTESIAN_POINT ( 'NONE',  ( 8.922933199037192509, -4.490180821391404287, 17.34886208192141765 ) ) ;
#1533 = CARTESIAN_POINT ( 'NONE',  ( -16.30827793483735988, 1.837501619626141780, 35.35714285714285410 ) ) ;
#1534 = DIRECTION ( 'NONE',  ( -1.000000000000000000, 0.000000000000000000, 0.000000000000000000 ) ) ;
#1535 = EDGE_CURVE ( 'NONE', #5109, #9801, #2466, .T. ) ;
#1536 = CARTESIAN_POINT ( 'NONE',  ( -5.543385399275643444, -15.44746603149420494, 20.07546914105500591 ) ) ;
#1537 = CARTESIAN_POINT ( 'NONE',  ( 9.383039235653818366, -1.486127417882130208, 1.200000000000034373 ) ) ;
#1538 = CARTESIAN_POINT ( 'NONE',  ( -13.82664651025767100, 8.841785722321537477, 21.78975485534072476 ) ) ;
#1539 = CARTESIAN_POINT ( 'NONE',  ( 11.60466159355862104, 11.60466159355875071, 19.50000000000000355 ) ) ;
#1540 = LINE ( 'NONE', #4687, #8260 ) ;
#1541 = VERTEX_POINT ( 'NONE', #8047 ) ;
#1542 = DIRECTION ( 'NONE',  ( 0.000000000000000000, -8.191099868251446680E-34, -1.000000000000000000 ) ) ;
#1543 = CARTESIAN_POINT ( 'NONE',  ( 13.89598863503045933, -8.731428362939032795, 38.78571428571429180 ) ) ;
#1544 =( LENGTH_UNIT ( ) NAMED_UNIT ( * ) SI_UNIT ( .MILLI., .METRE. ) );
#1545 = CARTESIAN_POINT ( 'NONE',  ( 9.333916720356675967, 4.809394265263123636, 10.89886208192140771 ) ) ;
#1546 = CARTESIAN_POINT ( 'NONE',  ( -8.512513224245306986, -13.54758718765259218, 4.285714285714288252 ) ) ;
#1547 = CARTESIAN_POINT ( 'NONE',  ( -11.60466159355861926, -11.60466159355875249, 4.500000000000005329 ) ) ;
#1548 = ITEM_DEFINED_TRANSFORMATION ( 'NONE', 'NONE', #8058,  #3995 ) ;
#1549 = CARTESIAN_POINT ( 'NONE',  ( 12.15899005565164792, -7.639999817571654361, 32.78571428571429180 ) ) ;
#1550 = CARTESIAN_POINT ( 'NONE',  ( -10.24623928997352351, -10.06191849875416899, 32.50404056962644006 ) ) ;
#1551 = CARTESIAN_POINT ( 'NONE',  ( 9.865911304835478290, 1.562606840307950273, 13.04999999999999538 ) ) ;
#1552 = CARTESIAN_POINT ( 'NONE',  ( -9.837026868206066865, 5.012215536711413399, 14.84999999999999787 ) ) ;
#1553 = ORIENTED_EDGE ( 'NONE', *, *, #2011, .T. ) ;
#1554 = CARTESIAN_POINT ( 'NONE',  ( -4.742819248065502258, -13.55419868402813677, 4.071428571428569398 ) ) ;
#1555 = ORIENTED_EDGE ( 'NONE', *, *, #7726, .T. ) ;
#1556 = CARTESIAN_POINT ( 'NONE',  ( 6.717514421272239744, -6.717514421272154479, 19.50000000000001776 ) ) ;
#1557 = CARTESIAN_POINT ( 'NONE',  ( -5.404401153735176599, 15.06016580658422477, 26.42453085894499765 ) ) ;
#1558 = CARTESIAN_POINT ( 'NONE',  ( 13.54758718765249803, 8.512513224245457977, 1.714285714285716855 ) ) ;
#1559 = CARTESIAN_POINT ( 'NONE',  ( -5.297344310588352201, -15.53355953199867301, 30.06738800180214355 ) ) ;
#1560 = DIRECTION ( 'NONE',  ( 1.000000000000000000, 0.000000000000000000, 0.000000000000000000 ) ) ;
#1561 = CARTESIAN_POINT ( 'NONE',  ( 9.837026868206066865, -5.012215536711392083, 1.350000000000015188 ) ) ;
#1562 = CARTESIAN_POINT ( 'NONE',  ( 4.623906867372411078, -13.21436662431711717, 3.428571428571426605 ) ) ;
#1563 = AXIS2_PLACEMENT_3D ( 'NONE', #520, #6802, #6597 ) ;
#1564 = CARTESIAN_POINT ( 'NONE',  ( 8.731428362939190890, -13.89598863503036164, 33.21428571428571530 ) ) ;
#1565 = ORIENTED_EDGE ( 'NONE', *, *, #2537, .F. ) ;
#1566 = CARTESIAN_POINT ( 'NONE',  ( -11.40355824106246807, 11.22385875690704715, 49.99595943037357415 ) ) ;
#1567 = CARTESIAN_POINT ( 'NONE',  ( 9.837026868206070418, -5.012215536711391195, 4.350000000000036948 ) ) ;
#1568 = CARTESIAN_POINT ( 'NONE',  ( 5.420364854932001819, 15.49051278174644430, 13.07142857142857295 ) ) ;
#1569 = DIRECTION ( 'NONE',  ( 0.000000000000000000, 0.000000000000000000, -1.000000000000000000 ) ) ;
#1570 = CARTESIAN_POINT ( 'NONE',  ( -4.743843029824828861, 13.17239914596749450, 26.42453085894499765 ) ) ;
#1571 = CARTESIAN_POINT ( 'NONE',  ( 7.390897758835871301, -7.458344646081624063, 3.501137918078585987 ) ) ;
#1572 = CARTESIAN_POINT ( 'NONE',  ( 8.877401133907127928, -4.579542530753017537, 18.35113791807858519 ) ) ;
#1573 = CARTESIAN_POINT ( 'NONE',  ( -163.3797476145753365, -1.420181920198508418, 12.92257903765585247 ) ) ;
#1574 = CARTESIAN_POINT ( 'NONE',  ( 10.24623928997352884, 10.06191849875416899, -0.4959594303735606058 ) ) ;
#1575 = CARTESIAN_POINT ( 'NONE',  ( 1.693770420379222319, 13.89774397934251837, 16.86118342676929061 ) ) ;
#1576 = ORIENTED_EDGE ( 'NONE', *, *, #3511, .F. ) ;
#1577 = CARTESIAN_POINT ( 'NONE',  ( -70.00000000000001421, 0.000000000000000000, 0.000000000000000000 ) ) ;
#1578 = CARTESIAN_POINT ( 'NONE',  ( 8.512513224245308763, 13.54758718765259040, 37.28571428571429180 ) ) ;
#1579 = CARTESIAN_POINT ( 'NONE',  ( 0.000000000000000000, 0.000000000000000000, 0.000000000000000000 ) ) ;
#1580 = CARTESIAN_POINT ( 'NONE',  ( -68.00000000000001421, 8.500000000000000000, 0.000000000000000000 ) ) ;
#1581 = CARTESIAN_POINT ( 'NONE',  ( 7.063212654743467489, 7.063212654743559860, 18.74999999999998934 ) ) ;
#1582 = CARTESIAN_POINT ( 'NONE',  ( -6.751237864895158758, 6.683790977649261222, 18.99886208192142334 ) ) ;
#1583 = CARTESIAN_POINT ( 'NONE',  ( -15.89939535829186923, -1.791431617653016062, 35.14285714285713880 ) ) ;
#1584 = CARTESIAN_POINT ( 'NONE',  ( -68.00000000000002842, 1.004210375300829674E-15, -8.200000000000001066 ) ) ;
#1585 = CARTESIAN_POINT ( 'NONE',  ( -13.61519076058348254, -8.404922754268771001, 32.71832628391215536 ) ) ;
#1586 = CARTESIAN_POINT ( 'NONE',  ( -158.0000000000000284, -7.514081744949122117E-15, 0.000000000000000000 ) ) ;
#1587 = CARTESIAN_POINT ( 'NONE',  ( 15.53355953199861794, 5.297344310588528060, 29.93261199819786356 ) ) ;
#1588 = CARTESIAN_POINT ( 'NONE',  ( -13.54758718765249625, -8.512513224245459753, 16.71428571428571530 ) ) ;
#1589 = DIRECTION ( 'NONE',  ( -1.000000000000000000, -0.000000000000000000, -0.000000000000000000 ) ) ;
#1590 = CARTESIAN_POINT ( 'NONE',  ( 5.284464991282756152, -15.10213328493384743, 3.428571428571426605 ) ) ;
#1591 =( NAMED_UNIT ( * ) PLANE_ANGLE_UNIT ( ) SI_UNIT ( $, .RADIAN. ) );
#1592 =( NAMED_UNIT ( * ) PLANE_ANGLE_UNIT ( ) SI_UNIT ( $, .RADIAN. ) );
#1593 = CARTESIAN_POINT ( 'NONE',  ( 1.689666864740335894, -10.36326688006720786, 5.798862081921429379 ) ) ;
#1594 = CARTESIAN_POINT ( 'NONE',  ( 10.24623928997352884, 10.06191849875416899, 41.50404056962644006 ) ) ;
#1595 = CARTESIAN_POINT ( 'NONE',  ( 15.49051278174638036, 5.420364854932175014, 13.92857142857143238 ) ) ;
#1596 = SHAPE_DEFINITION_REPRESENTATION ( #1956, #789 ) ;
#1597 = CARTESIAN_POINT ( 'NONE',  ( 9.899494936611718643, -9.899494936611608509, 39.00000000000000000 ) ) ;
#1598 = ADVANCED_FACE ( 'NONE', ( #9712 ), #1169, .T. ) ;
#1599 = CARTESIAN_POINT ( 'NONE',  ( -13.17239914596754424, 4.743843029824683200, 39.57546914105500946 ) ) ;
#1600 = CARTESIAN_POINT ( 'NONE',  ( -7.063212654743467489, -7.063212654743533214, 14.25000000000001421 ) ) ;
#1601 = CARTESIAN_POINT ( 'NONE',  ( -1.642561882922479732, 10.37072757624895303, 18.29999999999998295 ) ) ;
#1602 = ORIENTED_EDGE ( 'NONE', *, *, #7750, .F. ) ;
#1603 = CARTESIAN_POINT ( 'NONE',  ( -1.567502665446231180, -13.91197093850540334, 9.857142857142855874 ) ) ;
#1604 = LINE ( 'NONE', #3300, #3661 ) ;
#1605 = CARTESIAN_POINT ( 'NONE',  ( -13.96533075980324234, 8.621071003556515677, 31.78167371608784819 ) ) ;
#1606 = CARTESIAN_POINT ( 'NONE',  ( 16.30827793483735633, -1.837501619626142890, 20.35714285714285765 ) ) ;
#1607 = CARTESIAN_POINT ( 'NONE',  ( 1.967016585148662289, -16.29368510291087091, 23.63881657323070939 ) ) ;
#1608 = CARTESIAN_POINT ( 'NONE',  ( 5.012215536711511987, -9.837026868205999364, 1.650000000000006128 ) ) ;
#1609 = CARTESIAN_POINT ( 'NONE',  ( -10.37072757624895836, 1.642561882922381145, 5.700000000000038369 ) ) ;
#1610 = CARTESIAN_POINT ( 'NONE',  ( 56.99999999999997158, 9.797174393178825657E-16, -8.000000000000000000 ) ) ;
#1611 =( LENGTH_UNIT ( ) NAMED_UNIT ( * ) SI_UNIT ( .MILLI., .METRE. ) );
#1612 = CARTESIAN_POINT ( 'NONE',  ( 1.837501619626330074, -16.30827793483733501, 33.64285714285715301 ) ) ;
#1613 = VERTEX_POINT ( 'NONE', #2001 ) ;
#1614 = CARTESIAN_POINT ( 'NONE',  ( -4.766900247265192014, -9.355568503977876205, 17.10000000000000497 ) ) ;
#1615 = CARTESIAN_POINT ( 'NONE',  ( -8.512513224245306986, -13.54758718765259218, 10.28571428571428648 ) ) ;
#1616 = CARTESIAN_POINT ( 'NONE',  ( -168.0000000000000284, -2.363368035607157783E-15, 0.000000000000000000 ) ) ;
#1617 = CARTESIAN_POINT ( 'NONE',  ( -4.743843029824828861, 13.17239914596749450, 32.42453085894499054 ) ) ;
#1618 = CARTESIAN_POINT ( 'NONE',  ( -4.967534682030703586, 9.859792900771061852, 5.151137918078567246 ) ) ;
#1619 = CARTESIAN_POINT ( 'NONE',  ( 1.439022436064387511, -9.390499931835512015, 9.801137918078557831 ) ) ;
#1620 = LINE ( 'NONE', #4871, #1332 ) ;
#1621 = CARTESIAN_POINT ( 'NONE',  ( -11.92174236212692051, -7.340858601238089420, 2.718326283912150476 ) ) ;
#1622 = EDGE_CURVE ( 'NONE', #5319, #5655, #405, .T. ) ;
#1623 = ORIENTED_EDGE ( 'NONE', *, *, #5748, .T. ) ;
#1624 = CARTESIAN_POINT ( 'NONE',  ( -108.0000000000000284, 0.000000000000000000, 0.000000000000000000 ) ) ;
#1625 = CARTESIAN_POINT ( 'NONE',  ( 10.03895970123120307, 12.58845729673829972, 49.39149694378009769 ) ) ;
#1626 = AXIS2_PLACEMENT_3D ( 'NONE', #4740, #7887, #7113 ) ;
#1627 = DIRECTION ( 'NONE',  ( -0.000000000000000000, 0.000000000000000000, 1.000000000000000000 ) ) ;
#1628 = CARTESIAN_POINT ( 'NONE',  ( 2.000000000000001776, 0.000000000000000000, 0.000000000000000000 ) ) ;
#1629 = CARTESIAN_POINT ( 'NONE',  ( 1.562606840307832368, 9.865911304835510265, 15.44999999999997797 ) ) ;
#1630 = CARTESIAN_POINT ( 'NONE',  ( -9.383039235653820143, 1.486127417882155521, 5.700000000000038369 ) ) ;
#1631 = DIRECTION ( 'NONE',  ( 1.000000000000000000, 4.755747939841215952E-17, -0.000000000000000000 ) ) ;
#1632 = CARTESIAN_POINT ( 'NONE',  ( -15.06016580658428694, 5.404401153735006957, 27.57546914105500946 ) ) ;
#1633 = CARTESIAN_POINT ( 'NONE',  ( -8.464561979789474222, -4.312909747525729642, 2.400000000000013234 ) ) ;
#1634 = CARTESIAN_POINT ( 'NONE',  ( -1.707986654103994528, 16.32287076676380266, 28.64689771248357886 ) ) ;
#1635 = EDGE_LOOP ( 'NONE', ( #7592, #4013, #4601, #9629 ) ) ;
#1636 = CARTESIAN_POINT ( 'NONE',  ( -5.284464991282755264, 15.10213328493384743, 30.42857142857143060 ) ) ;
#1637 = CARTESIAN_POINT ( 'NONE',  ( -170.0000000000000284, -1.448262861947153525E-15, 0.000000000000000000 ) ) ;
#1638 = CARTESIAN_POINT ( 'NONE',  ( -5.284464991282755264, 15.10213328493384743, 6.428571428571429713 ) ) ;
#1639 = FACE_OUTER_BOUND ( 'NONE', #6518, .T. ) ;
#1640 = SURFACE_SIDE_STYLE ('',( #8718 ) ) ;
#1641 = CARTESIAN_POINT ( 'NONE',  ( 1.533232399700100945, -9.375578539472073203, 2.798862081921426714 ) ) ;
#1642 = UNCERTAINTY_MEASURE_WITH_UNIT (LENGTH_MEASURE( 1.000000000000000082E-05 ), #1433, 'distance_accuracy_value', 'NONE');
#1643 = CARTESIAN_POINT ( 'NONE',  ( 1.677562661911645714, 10.91227292449347175, 7.448862081921427070 ) ) ;
#1644 = CARTESIAN_POINT ( 'NONE',  ( -1.917699372585823570, -15.88516839912900558, 1.861183426769295490 ) ) ;
#1645 = CARTESIAN_POINT ( 'NONE',  ( -11.31370849898482156, 11.31370849898469544, 18.00000000000000355 ) ) ;
#1646 = CARTESIAN_POINT ( 'NONE',  ( -13.91197093850538380, -1.567502665446387278, 41.14285714285714590 ) ) ;
#1647 = CARTESIAN_POINT ( 'NONE',  ( -10.24623928997352351, -10.06191849875416899, 38.50404056962644006 ) ) ;
#1648 = CARTESIAN_POINT ( 'NONE',  ( -4.503970704919988854, 13.25633410266674517, 34.43261199819786356 ) ) ;
#1649 = CARTESIAN_POINT ( 'NONE',  ( 1.562606840307832146, 9.865911304835508489, 9.449999999999992184 ) ) ;
#1650 = CARTESIAN_POINT ( 'NONE',  ( -10.90442828429183919, -1.727091770866654663, 14.55000000000000249 ) ) ;
#1651 = VERTEX_POINT ( 'NONE', #9037 ) ;
#1652 = CARTESIAN_POINT ( 'NONE',  ( 4.623906867372411078, -13.21436662431711717, 3.428571428571426605 ) ) ;
#1653 = CARTESIAN_POINT ( 'NONE',  ( 4.200000000000009059, 0.000000000000000000, 0.000000000000000000 ) ) ;
#1654 = CARTESIAN_POINT ( 'NONE',  ( -11.31370849898482156, 11.31370849898469544, 11.99999999999999645 ) ) ;
#1655 = CARTESIAN_POINT ( 'NONE',  ( -1.665163862719845067, -15.91362231745477374, 41.85310228751642825 ) ) ;
#1656 = CARTESIAN_POINT ( 'NONE',  ( -9.837026868206066865, 5.012215536711413399, 2.849999999999968114 ) ) ;
#1657 = CARTESIAN_POINT ( 'NONE',  ( 5.012215536711511987, -9.837026868205999364, 4.650000000000026112 ) ) ;
#1658 = CARTESIAN_POINT ( 'NONE',  ( 10.15407889436379030, 10.15407889436390221, 1.500000000000003553 ) ) ;
#1659 = ADVANCED_FACE ( 'NONE', ( #2101 ), #7385, .T. ) ;
#1660 = EDGE_CURVE ( 'NONE', #7847, #3628, #10060, .T. ) ;
#1661 = CIRCLE ( 'NONE', #8917, 3.299999999999999822 ) ;
#1662 = AXIS2_PLACEMENT_3D ( 'NONE', #3535, #4306, #3624 ) ;
#1663 = ORIENTED_EDGE ( 'NONE', *, *, #6058, .F. ) ;
#1664 = CARTESIAN_POINT ( 'NONE',  ( 4.743843029824831525, -13.17239914596749095, 11.42453085894499587 ) ) ;
#1665 = CARTESIAN_POINT ( 'NONE',  ( -5.012215536711508435, 9.837026868206027785, 15.14999999999998614 ) ) ;
#1666 = FACE_OUTER_BOUND ( 'NONE', #313, .T. ) ;
#1667 = CARTESIAN_POINT ( 'NONE',  ( -1.441234910513241818, -13.92619789766829008, 23.85310228751642825 ) ) ;
#1668 = CARTESIAN_POINT ( 'NONE',  ( 1.595456901104624459, -10.37818827243065201, 3.801137918078595135 ) ) ;
#1670 = AXIS2_PLACEMENT_3D ( 'NONE', #4015, #7834, #865 ) ;
#1669 = CARTESIAN_POINT ( 'NONE',  ( 6.683790977649321619, -6.751237864895082375, 12.50113791807859265 ) ) ;
#1671 = AXIS2_PLACEMENT_3D ( 'NONE', #6938, #5350, #8502 ) ;
#1672 = AXIS2_PLACEMENT_3D ( 'NONE', #4974, #3942, #9683 ) ;
#1673 = DIRECTION ( 'NONE',  ( -1.000000000000000000, -0.000000000000000000, -0.000000000000000000 ) ) ;
#1674 = CARTESIAN_POINT ( 'NONE',  ( 13.17239914596754424, -4.743843029824685864, 0.5754691410550027975 ) ) ;
#1675 = CARTESIAN_POINT ( 'NONE',  ( -1.693770420379220099, -13.89774397934251837, 7.861183426769288829 ) ) ;
#1676 = AXIS2_PLACEMENT_3D ( 'NONE', #7871, #8656, #7781 ) ;
#1677 = PRESENTATION_LAYER_ASSIGNMENT (  '', '', ( #9437 ) ) ;
#1678 = CARTESIAN_POINT ( 'NONE',  ( -70.00000000000001421, 0.000000000000000000, 16.00000000000000000 ) ) ;
#1679 =( GEOMETRIC_REPRESENTATION_CONTEXT ( 3 ) GLOBAL_UNCERTAINTY_ASSIGNED_CONTEXT ( ( #398 ) ) GLOBAL_UNIT_ASSIGNED_CONTEXT ( ( #6272, #5511, #4738 ) ) REPRESENTATION_CONTEXT ( 'NONE', 'WORKASPACE' ) );
#1680 =( GEOMETRIC_REPRESENTATION_CONTEXT ( 3 ) GLOBAL_UNCERTAINTY_ASSIGNED_CONTEXT ( ( #7319 ) ) GLOBAL_UNIT_ASSIGNED_CONTEXT ( ( #1172, #8987, #349 ) ) REPRESENTATION_CONTEXT ( 'NONE', 'WORKASPACE' ) );
#1681 = CARTESIAN_POINT ( 'NONE',  ( -16.30827793483735988, 1.837501619626141780, 41.35714285714286120 ) ) ;
#1682 = CARTESIAN_POINT ( 'NONE',  ( -166.0067307485407184, -1.311714535335565923, 12.93379411699749681 ) ) ;
#1683 = DIRECTION ( 'NONE',  ( -1.000000000000000000, 0.000000000000000000, 0.000000000000000000 ) ) ;
#1684 = CARTESIAN_POINT ( 'NONE',  ( 6.717514421272239744, -6.717514421272154479, 13.50000000000001243 ) ) ;
#1685 = CARTESIAN_POINT ( 'NONE',  ( 1.562606840307832368, 9.865911304835510265, 9.449999999999988631 ) ) ;
#1686 = ADVANCED_FACE ( 'NONE', ( #2972 ), #9038, .T. ) ;
#1687 = CARTESIAN_POINT ( 'NONE',  ( -165.5651189253971722, 2.093213258176506386, 12.83083170865760181 ) ) ;
#1688 = CARTESIAN_POINT ( 'NONE',  ( 8.620103694221997515, 13.47998361472160767, 29.28975485534071765 ) ) ;
#1689 = CARTESIAN_POINT ( 'NONE',  ( 4.534861676072321046, -8.900167166472098046, 4.650000000000027001 ) ) ;
#1690 = STYLED_ITEM ( 'NONE', ( #7394 ), #2769 ) ;
#1691 = CARTESIAN_POINT ( 'NONE',  ( -5.164528828830334817, 15.14410076328347543, 40.43261199819787066 ) ) ;
#1692 = VERTEX_POINT ( 'NONE', #7477 ) ;
#1693 = CARTESIAN_POINT ( 'NONE',  ( 5.420364854932001819, 15.49051278174644430, 31.07142857142857295 ) ) ;
#1694 = CARTESIAN_POINT ( 'NONE',  ( 3.926188687689436296, 14.48606370741319083, 1.336143574210037107E-16 ) ) ;
#1695 = CARTESIAN_POINT ( 'NONE',  ( -108.0000000000000284, 0.000000000000000000, 0.000000000000000000 ) ) ;
#1696 = CARTESIAN_POINT ( 'NONE',  ( 1.533232399700100945, -9.375578539472067874, 5.798862081921429379 ) ) ;
#1697 = CARTESIAN_POINT ( 'NONE',  ( 1.689666864740335894, -10.36326688006720786, 14.79886208192143471 ) ) ;
#1698 = CARTESIAN_POINT ( 'NONE',  ( -15.53355953199861794, -5.297344310588530725, 2.932611998197868886 ) ) ;
#1699 = CARTESIAN_POINT ( 'NONE',  ( -13.89598863503046111, 8.731428362939027465, 11.78571428571428115 ) ) ;
#1700 = CARTESIAN_POINT ( 'NONE',  ( 4.742819248065502258, 13.55419868402813499, 43.07142857142857650 ) ) ;
#1701 = CARTESIAN_POINT ( 'NONE',  ( -13.17239914596754424, 4.743843029824683200, 45.57546914105501656 ) ) ;
#1702 = CARTESIAN_POINT ( 'NONE',  ( -10.15407889436378852, -10.15407889436390576, 4.500000000000005329 ) ) ;
#1703 = CARTESIAN_POINT ( 'NONE',  ( -9.865911304835474738, -1.562606840307925626, 14.55000000000000604 ) ) ;
#1704 = CARTESIAN_POINT ( 'NONE',  ( 7.771249796623105333, 7.842167650704658932, 10.74886208192140913 ) ) ;
#1705 = VERTEX_POINT ( 'NONE', #2871 ) ;
#1706 = CARTESIAN_POINT ( 'NONE',  ( 1.567502665446232957, 13.91197093850540156, 6.857142857142860315 ) ) ;
#1707 = ORIENTED_EDGE ( 'NONE', *, *, #6644, .F. ) ;
#1708 = DIRECTION ( 'NONE',  ( 0.000000000000000000, 6.338944243255235518E-49, -1.000000000000000000 ) ) ;
#1709 = CARTESIAN_POINT ( 'NONE',  ( -15.49051278174637858, -5.420364854932175014, 10.92857142857143060 ) ) ;
#1710 = VECTOR ( 'NONE', #8816, 1000.000000000000000 ) ;
#1711 = CARTESIAN_POINT ( 'NONE',  ( -8.841785722321695573, 13.82664651025757152, 44.21024514465928235 ) ) ;
#1712 =( REPRESENTATION_RELATIONSHIP ('NONE','NONE', #58, #789 ) REPRESENTATION_RELATIONSHIP_WITH_TRANSFORMATION ( #4025 )SHAPE_REPRESENTATION_RELATIONSHIP( ) );
#1713 = CARTESIAN_POINT ( 'NONE',  ( -5.012215536711506658, 9.837026868206027785, 12.14999999999996305 ) ) ;
#1714 = CARTESIAN_POINT ( 'NONE',  ( -4.766900247265192014, -9.355568503977876205, 2.099999999999990763 ) ) ;
#1715 = DIRECTION ( 'NONE',  ( 0.000000000000000000, -1.000000000000000000, 1.332267629550187849E-15 ) ) ;
#1716 = AXIS2_PLACEMENT_3D ( 'NONE', #7873, #7733, #6362 ) ;
#1717 = VERTEX_POINT ( 'NONE', #1177 ) ;
#1718 = CARTESIAN_POINT ( 'NONE',  ( -4.619798703721853528, -13.59724543428036725, 18.06738800180213644 ) ) ;
#1719 = CARTESIAN_POINT ( 'NONE',  ( 9.355568503977840678, 4.766900247265305701, 12.90000000000002345 ) ) ;
#1720 = CARTESIAN_POINT ( 'NONE',  ( -163.4027093359710534, 0.4274795813385452448, 12.99339846045314850 ) ) ;
#1721 = CARTESIAN_POINT ( 'NONE',  ( 1.791431617652837316, 15.89939535829188877, 36.85714285714286120 ) ) ;
#1722 = CARTESIAN_POINT ( 'NONE',  ( 1.441234910513245149, 13.92619789766829008, 38.85310228751641404 ) ) ;
#1723 = CARTESIAN_POINT ( 'NONE',  ( 9.377220287599001836, 4.724406229267492208, 11.90113791807857702 ) ) ;
#1724 = CARTESIAN_POINT ( 'NONE',  ( -6.683790977649319842, 6.751237864895101026, 17.00113791807859442 ) ) ;
#1725 = CIRCLE ( 'NONE', #5513, 13.00000000000000000 ) ;
#1726 = CARTESIAN_POINT ( 'NONE',  ( -165.0000000000000284, -1.734723475976807094E-15, 3.000000000000002665 ) ) ;
#1727 = CARTESIAN_POINT ( 'NONE',  ( -13.59724543428031573, -4.619798703722008959, 8.932611998197868886 ) ) ;
#1728 = CARTESIAN_POINT ( 'NONE',  ( -7.556039541191334585, -11.78653521626503320, 14.28975485534072298 ) ) ;
#1729 = FACE_OUTER_BOUND ( 'NONE', #8740, .T. ) ;
#1730 = CARTESIAN_POINT ( 'NONE',  ( 1.967016585148662289, -16.29368510291087091, 5.638816573230711171 ) ) ;
#1731 = CARTESIAN_POINT ( 'NONE',  ( -165.2804454449952516, -2.136238053246409141, 14.84712918936600623 ) ) ;
#1732 = CARTESIAN_POINT ( 'NONE',  ( -9.383039235653820143, 1.486127417882154411, 14.69999999999999041 ) ) ;
#1733 = CARTESIAN_POINT ( 'NONE',  ( 6.717514421272239744, -6.717514421272154479, 4.500000000000003553 ) ) ;
#1734 = CARTESIAN_POINT ( 'NONE',  ( -160.0000000000000284, -7.609196703745946707E-15, 0.000000000000000000 ) ) ;
#1735 = CYLINDRICAL_SURFACE ( 'NONE', #8585, 2.000000000000000888 ) ;
#1736 = CARTESIAN_POINT ( 'NONE',  ( -15.53355953199861794, -5.297344310588530725, 32.93261199819787777 ) ) ;
#1737 = EDGE_LOOP ( 'NONE', ( #9620, #4128, #5037, #10200 ) ) ;
#1738 = CARTESIAN_POINT ( 'NONE',  ( 15.89939535829187278, 1.791431617653015174, 26.14285714285714590 ) ) ;
#1739 = CARTESIAN_POINT ( 'NONE',  ( 3.523512929767037338, 14.36041041362159554, 8.096169431371280833E-17 ) ) ;
#1740 = CARTESIAN_POINT ( 'NONE',  ( 11.60466159355862104, 11.60466159355875071, 7.500000000000005329 ) ) ;
#1741 = CARTESIAN_POINT ( 'NONE',  ( -9.858066664633883036, -1.612135949262833101, 9.548862081921404510 ) ) ;
#1742 = CARTESIAN_POINT ( 'NONE',  ( 1.513077731352925115, 9.873755945037103743, 1.448862081921441947 ) ) ;
#1743 = UNCERTAINTY_MEASURE_WITH_UNIT (LENGTH_MEASURE( 1.000000000000000082E-05 ), #365, 'distance_accuracy_value', 'NONE');
#1744 = CARTESIAN_POINT ( 'NONE',  ( -11.22385875690717327, 11.40355824106234550, -1.995959430373561272 ) ) ;
#1745 = ADVANCED_FACE ( 'NONE', ( #3549 ), #5914, .F. ) ;
#1746 = CARTESIAN_POINT ( 'NONE',  ( -1.837501619626328297, 16.30827793483733856, 12.64285714285714235 ) ) ;
#1747 = CARTESIAN_POINT ( 'NONE',  ( 13.21436662431716869, -4.623906867372263640, 32.57142857142856940 ) ) ;
#1748 = CARTESIAN_POINT ( 'NONE',  ( 5.543385399275644332, 15.44746603149420494, -0.9245308589449906522 ) ) ;
#1749 = CARTESIAN_POINT ( 'NONE',  ( -4.623906867372410190, 13.21436662431711895, 12.42857142857142705 ) ) ;
#1750 = LINE ( 'NONE', #5814, #7591 ) ;
#1751 = CARTESIAN_POINT ( 'NONE',  ( -1.689666864740335228, 10.36326688006723451, 7.298862081921430267 ) ) ;
#1752 = ORIENTED_EDGE ( 'NONE', *, *, #6023, .F. ) ;
#1753 = CARTESIAN_POINT ( 'NONE',  ( 7.448449071214646722, 11.85413878919601594, 1.285714285714285809 ) ) ;
#1754 = DIRECTION ( 'NONE',  ( 1.000000000000000000, 4.755747939841215952E-17, -0.000000000000000000 ) ) ;
#1755 = CARTESIAN_POINT ( 'NONE',  ( -11.31370849898482156, 11.31370849898469544, 24.00000000000000000 ) ) ;
#1756 = CARTESIAN_POINT ( 'NONE',  ( 15.44746603149413922, 5.543385399275817527, 39.92453085894499054 ) ) ;
#1757 = CARTESIAN_POINT ( 'NONE',  ( 9.355568503977840678, 4.766900247265305701, 6.899999999999961275 ) ) ;
#1758 = CARTESIAN_POINT ( 'NONE',  ( 1.642561882922480621, -10.37072757624891750, 7.800000000000029132 ) ) ;
#1759 = CARTESIAN_POINT ( 'NONE',  ( 9.899494936611718643, -9.899494936611608509, 3.000000000000002665 ) ) ;
#1760 = ORIENTED_EDGE ( 'NONE', *, *, #4876, .T. ) ;
#1761 = CARTESIAN_POINT ( 'NONE',  ( 7.750357176954296712, -12.08964793087877787, 11.21024514465928235 ) ) ;
#1762 = CARTESIAN_POINT ( 'NONE',  ( -1.642561882922479732, 10.37072757624895303, 15.29999999999997939 ) ) ;
#1763 = LINE ( 'NONE', #9577, #3701 ) ;
#1764 = CARTESIAN_POINT ( 'NONE',  ( 7.340858601237956194, 11.92174236212700045, 39.28167371608785174 ) ) ;
#1765 = CARTESIAN_POINT ( 'NONE',  ( 7.842167650704563897, 7.771249796623202144, 11.75113791807857666 ) ) ;
#1766 = CARTESIAN_POINT ( 'NONE',  ( 9.375578539472099848, -1.533232399699987702, 12.20113791807854398 ) ) ;
#1767 = AXIS2_PLACEMENT_3D ( 'NONE', #5692, #8860, #1773 ) ;
#1768 = DIRECTION ( 'NONE',  ( -1.000000000000000000, -4.755747939841215952E-17, 0.000000000000000000 ) ) ;
#1769 = CARTESIAN_POINT ( 'NONE',  ( -4.865839792409144771, -13.51115193377589740, 14.07546914105500768 ) ) ;
#1770 =( NAMED_UNIT ( * ) PLANE_ANGLE_UNIT ( ) SI_UNIT ( $, .RADIAN. ) );
#1771 = CARTESIAN_POINT ( 'NONE',  ( -9.809645194534070356, 9.989344678689256796, 16.00404056962643651 ) ) ;
#1772 = ORIENTED_EDGE ( 'NONE', *, *, #967, .F. ) ;
#1773 = DIRECTION ( 'NONE',  ( 1.000000000000000000, 0.000000000000000000, 0.000000000000000000 ) ) ;
#1774 = CARTESIAN_POINT ( 'NONE',  ( -1.665163862719845067, -15.91362231745477374, 5.853102287516418478 ) ) ;
#1775 = CARTESIAN_POINT ( 'NONE',  ( -165.2175649311437837, -1.639125141419205622, 12.89626763964974465 ) ) ;
#1776 = DIRECTION ( 'NONE',  ( 0.000000000000000000, -6.338944243255235518E-49, 1.000000000000000000 ) ) ;
#1777 = CARTESIAN_POINT ( 'NONE',  ( -9.873755945037078874, -1.513077731353020594, 1.551137918078593803 ) ) ;
#1778 = CARTESIAN_POINT ( 'NONE',  ( -4.312909747525649706, -8.464561979789499091, 11.09999999999999787 ) ) ;
#1779 = DIRECTION ( 'NONE',  ( 0.000000000000000000, 1.000000000000000000, 0.000000000000000000 ) ) ;
#1780 = CARTESIAN_POINT ( 'NONE',  ( 11.69682198916835070, 11.51250119794901394, 23.50404056962643295 ) ) ;
#1781 = CARTESIAN_POINT ( 'NONE',  ( 4.623906867372411078, -13.21436662431711717, 33.42857142857143060 ) ) ;
#1782 = CARTESIAN_POINT ( 'NONE',  ( 16.29368510291089223, -1.967016585148476882, 36.36118342676930126 ) ) ;
#1783 = EDGE_CURVE ( 'NONE', #503, #6536, #171, .T. ) ;
#1784 = ORIENTED_EDGE ( 'NONE', *, *, #755, .F. ) ;
#1785 = CARTESIAN_POINT ( 'NONE',  ( 11.60466159355862104, 11.60466159355875071, 25.50000000000000711 ) ) ;
#1786 = DIRECTION ( 'NONE',  ( 1.000000000000000000, 0.000000000000000000, 0.000000000000000000 ) ) ;
#1787 = CARTESIAN_POINT ( 'NONE',  ( 1.791431617652837316, 15.89939535829188877, 12.85714285714285943 ) ) ;
#1788 = SURFACE_STYLE_FILL_AREA ( #392 ) ;
#1789 = DIRECTION ( 'NONE',  ( 1.000000000000000000, 4.755747939841215952E-17, -0.000000000000000000 ) ) ;
#1790 = CARTESIAN_POINT ( 'NONE',  ( 8.464561979789474222, 4.312909747525755400, 0.9000000000000119016 ) ) ;
#1791 = CARTESIAN_POINT ( 'NONE',  ( -1.689666864740335228, 10.36326688006722740, 13.29886208192143471 ) ) ;
#1792 = CARTESIAN_POINT ( 'NONE',  ( -1.707986654103994528, 16.32287076676380266, -1.353102287516420921 ) ) ;
#1793 = CARTESIAN_POINT ( 'NONE',  ( 1.837501619626330074, -16.30827793483733501, 9.642857142857147679 ) ) ;
#1794 = CARTESIAN_POINT ( 'NONE',  ( -4.623906867372410190, 13.21436662431711895, 48.42857142857143060 ) ) ;
#1795 = CARTESIAN_POINT ( 'NONE',  ( -7.556039541191334585, -11.78653521626503320, 38.28975485534072476 ) ) ;
#1796 = CARTESIAN_POINT ( 'NONE',  ( 13.21436662431716869, -4.623906867372263640, 14.57142857142856940 ) ) ;
#1797 = CARTESIAN_POINT ( 'NONE',  ( -7.458344646081709328, 7.390897758835799358, 12.99886208192142512 ) ) ;
#1798 = ORIENTED_EDGE ( 'NONE', *, *, #549, .T. ) ;
#1799 = CARTESIAN_POINT ( 'NONE',  ( -9.899494936611716867, 9.899494936611610285, 18.00000000000000355 ) ) ;
#1800 = EDGE_LOOP ( 'NONE', ( #7175, #1286 ) ) ;
#1801 = CARTESIAN_POINT ( 'NONE',  ( 2.000000000000001776, 0.8865213383407039016, -1.535500000000022958 ) ) ;
#1802 = CARTESIAN_POINT ( 'NONE',  ( 8.512513224245308763, 13.54758718765259040, 13.28571428571429003 ) ) ;
#1803 = CARTESIAN_POINT ( 'NONE',  ( -11.40355824106246807, 11.22385875690704715, 31.99595943037357060 ) ) ;
#1804 = CARTESIAN_POINT ( 'NONE',  ( 9.837026868206066865, -5.012215536711391195, 4.350000000000036948 ) ) ;
#1805 = CARTESIAN_POINT ( 'NONE',  ( -10.90442828429183919, -1.727091770866654663, 11.54999999999998295 ) ) ;
#1806 = ADVANCED_FACE ( 'NONE', ( #7936 ), #3077, .F. ) ;
#1807 = CARTESIAN_POINT ( 'NONE',  ( 13.91197093850538380, 1.567502665446386390, 14.14285714285714413 ) ) ;
#1808 = ORIENTED_EDGE ( 'NONE', *, *, #4409, .F. ) ;
#1809 = CARTESIAN_POINT ( 'NONE',  ( -4.743843029824828861, 13.17239914596749450, 14.42453085894499232 ) ) ;
#1810 = VERTEX_POINT ( 'NONE', #1486 ) ;
#1811 = CARTESIAN_POINT ( 'NONE',  ( -10.90442828429184274, -1.727091770866655107, 14.55000000000000604 ) ) ;
#1812 = CYLINDRICAL_SURFACE ( 'NONE', #2046, 13.00000000000000178 ) ;
#1813 = CARTESIAN_POINT ( 'NONE',  ( 13.51115193377584589, 4.865839792409294873, 39.92453085894499054 ) ) ;
#1814 = CARTESIAN_POINT ( 'NONE',  ( -9.377220287598998283, -4.724406229267462898, 16.40113791807857524 ) ) ;
#1815 = CARTESIAN_POINT ( 'NONE',  ( 1.776620879821457333, 10.89658364409028124, 8.451137918078549305 ) ) ;
#1816 = CARTESIAN_POINT ( 'NONE',  ( -5.986002070941136566, -13.58603705635637482, 0.000000000000000000 ) ) ;
#1817 = CARTESIAN_POINT ( 'NONE',  ( -14.25515036105622890, 1.737328882695209575, 15.36118342676929771 ) ) ;
#1818 = EDGE_CURVE ( 'NONE', #7986, #4850, #9758, .T. ) ;
#1819 = CARTESIAN_POINT ( 'NONE',  ( -14.25515036105622890, 1.737328882695209575, 21.36118342676929771 ) ) ;
#1820 = DIRECTION ( 'NONE',  ( 0.000000000000000000, -1.224646799147353207E-16, 1.000000000000000000 ) ) ;
#1821 = CARTESIAN_POINT ( 'NONE',  ( -5.297344310588352201, -15.53355953199867301, 12.06738800180214000 ) ) ;
#1822 = DIRECTION ( 'NONE',  ( -1.000000000000000000, -0.000000000000000000, -0.000000000000000000 ) ) ;
#1823 = FACE_OUTER_BOUND ( 'NONE', #750, .T. ) ;
#1824 = VECTOR ( 'NONE', #440, 1000.000000000000000 ) ;
#1825 = AXIS2_PLACEMENT_3D ( 'NONE', #3023, #603, #3749 ) ;
#1826 = AXIS2_PLACEMENT_3D ( 'NONE', #4668, #5385, #3735 ) ;
#1827 = CARTESIAN_POINT ( 'NONE',  ( 6.683790977649321619, -6.751237864895076157, 9.501137918078587319 ) ) ;
#1828 = CARTESIAN_POINT ( 'NONE',  ( -1.562606840307830591, -9.865911304835488949, 4.950000000000017053 ) ) ;
#1829 = CYLINDRICAL_SURFACE ( 'NONE', #3463, 16.00000000000000000 ) ;
#1830 = CARTESIAN_POINT ( 'NONE',  ( -10.15407889436378852, -10.15407889436390576, 28.50000000000001066 ) ) ;
#1831 = CARTESIAN_POINT ( 'NONE',  ( 8.620103694221997515, 13.47998361472160767, 41.28975485534072476 ) ) ;
#1832 = AXIS2_PLACEMENT_3D ( 'NONE', #1072, #7466, #8187 ) ;
#1833 = CIRCLE ( 'NONE', #2488, 8.000000000000000000 ) ;
#1834 = ORIENTED_EDGE ( 'NONE', *, *, #4659, .T. ) ;
#1835 = CARTESIAN_POINT ( 'NONE',  ( 8.512513224245308763, 13.54758718765259040, 31.28571428571428470 ) ) ;
#1836 = DIRECTION ( 'NONE',  ( 0.000000000000000000, -6.338944243255235518E-49, 1.000000000000000000 ) ) ;
#1837 = CARTESIAN_POINT ( 'NONE',  ( 13.54758718765249803, 8.512513224245457977, 19.71428571428571175 ) ) ;
#1838 = EDGE_CURVE ( 'NONE', #7160, #3093, #1412, .T. ) ;
#1839 =( LENGTH_UNIT ( ) NAMED_UNIT ( * ) SI_UNIT ( .MILLI., .METRE. ) );
#1840 = CARTESIAN_POINT ( 'NONE',  ( -8.464561979789474222, -4.312909747525729642, 2.400000000000013234 ) ) ;
#1841 = CARTESIAN_POINT ( 'NONE',  ( 7.027753727702739539, 7.098671581784288698, 1.748862081921432887 ) ) ;
#1842 = CONICAL_SURFACE ( 'NONE', #5792, 1.535500000000000087, 1.047197551196590748 ) ;
#1843 = SHAPE_REPRESENTATION ( 'small spring', ( #3995 ), #6704 ) ;
#1844 = UNCERTAINTY_MEASURE_WITH_UNIT (LENGTH_MEASURE( 1.000000000000000082E-05 ), #1839, 'distance_accuracy_value', 'NONE');
#1845 = CARTESIAN_POINT ( 'NONE',  ( 15.06016580658428694, -5.404401153735007846, 12.57546914105500768 ) ) ;
#1846 = CARTESIAN_POINT ( 'NONE',  ( -16.30827793483735988, 1.837501619626141780, 29.35714285714285765 ) ) ;
#1847 = FILL_AREA_STYLE ('',( #5710 ) ) ;
#1848 = CARTESIAN_POINT ( 'NONE',  ( 11.22385875690717683, -11.40355824106234373, 1.004040569626440726 ) ) ;
#1849 = CLOSED_SHELL ( 'NONE', ( #1340, #3482, #6215, #5630, #9440, #1745 ) ) ;
#1850 = CARTESIAN_POINT ( 'NONE',  ( -4.742819248065502258, -13.55419868402813677, 16.07142857142857650 ) ) ;
#1851 = CARTESIAN_POINT ( 'NONE',  ( 8.900167166472158442, -4.534861676072213577, 16.35000000000000853 ) ) ;
#1852 = CARTESIAN_POINT ( 'NONE',  ( 7.458344646081711105, -7.390897758835786036, 11.49886208192146775 ) ) ;
#1853 = ORIENTED_EDGE ( 'NONE', *, *, #3450, .T. ) ;
#1854 = CARTESIAN_POINT ( 'NONE',  ( 7.639999817571789364, -12.15899005565156266, 21.21428571428571885 ) ) ;
#1855 = CIRCLE ( 'NONE', #7631, 8.200000000000001066 ) ;
#1856 = CARTESIAN_POINT ( 'NONE',  ( 8.512513224245308763, 13.54758718765259040, 31.28571428571428470 ) ) ;
#1857 = CARTESIAN_POINT ( 'NONE',  ( 1.665163862719847732, 15.91362231745477374, 32.85310228751642114 ) ) ;
#1858 = CARTESIAN_POINT ( 'NONE',  ( 7.806708723663831506, 7.806708723663930982, 6.749999999999960032 ) ) ;
#1859 = CARTESIAN_POINT ( 'NONE',  ( 7.424621202458790314, -7.424621202458697944, 13.50000000000001243 ) ) ;
#1860 = CARTESIAN_POINT ( 'NONE',  ( -13.21436662431716869, 4.623906867372262752, 5.571428571428574728 ) ) ;
#1861 = ORIENTED_EDGE ( 'NONE', *, *, #8921, .T. ) ;
#1862 = CARTESIAN_POINT ( 'NONE',  ( -4.619798703721853528, -13.59724543428036725, 24.06738800180213644 ) ) ;
#1863 = ORIENTED_EDGE ( 'NONE', *, *, #1508, .T. ) ;
#1864 = DIRECTION ( 'NONE',  ( -1.000000000000000000, -0.000000000000000000, -0.000000000000000000 ) ) ;
#1865 = VECTOR ( 'NONE', #9017, 1000.000000000000000 ) ;
#1866 = CARTESIAN_POINT ( 'NONE',  ( -164.7839123519666487, 1.649920478573665195, 12.89487349378784664 ) ) ;
#1867 = CARTESIAN_POINT ( 'NONE',  ( -7.340858601237953529, -11.92174236212700222, 36.28167371608785174 ) ) ;
#1868 = CARTESIAN_POINT ( 'NONE',  ( -1.595456901104623348, 10.37818827243067155, 14.30113791807856316 ) ) ;
#1869 = CARTESIAN_POINT ( 'NONE',  ( -7.390897758835869524, 7.458344646081637386, 2.001137918078543354 ) ) ;
#1870 = EDGE_CURVE ( 'NONE', #5718, #951, #10115, .T. ) ;
#1871 = DIRECTION ( 'NONE',  ( 0.000000000000000000, -1.000000000000000000, 0.000000000000000000 ) ) ;
#1872 = CARTESIAN_POINT ( 'NONE',  ( -7.556039541191334585, -11.78653521626503320, 20.28975485534072121 ) ) ;
#1873 = SURFACE_SIDE_STYLE ('',( #8961 ) ) ;
#1874 = PRODUCT ( 'round tube', 'round tube', '', ( #512 ) ) ;
#1875 = CARTESIAN_POINT ( 'NONE',  ( 10.90442828429183919, 1.727091770866679532, 10.05000000000002736 ) ) ;
#1876 = CARTESIAN_POINT ( 'NONE',  ( -13.47998361472151174, -8.620103694222146729, 42.71024514465928235 ) ) ;
#1877 = ORIENTED_EDGE ( 'NONE', *, *, #1055, .T. ) ;
#1878 = CARTESIAN_POINT ( 'NONE',  ( -6.655197264005453306, 14.52795920839829513, 48.73000000000004661 ) ) ;
#1879 = CARTESIAN_POINT ( 'NONE',  ( -5.284464991282755264, 15.10213328493384743, 18.42857142857143415 ) ) ;
#1880 = CARTESIAN_POINT ( 'NONE',  ( 16.32287076676382043, -1.707986654103810897, 10.35310228751642292 ) ) ;
#1881 = DIRECTION ( 'NONE',  ( -5.603403109029596495E-32, -1.224646799147353207E-16, 1.000000000000000000 ) ) ;
#1882 = CARTESIAN_POINT ( 'NONE',  ( -167.1500000000000341, -1.102909754258692077E-14, 15.00000000000000000 ) ) ;
#1883 = CARTESIAN_POINT ( 'NONE',  ( 9.873755945037075321, 1.513077731353044131, 6.051137918078538291 ) ) ;
#1884 = CARTESIAN_POINT ( 'NONE',  ( -9.383039235653820143, 1.486127417882154411, 14.69999999999999041 ) ) ;
#1885 = CARTESIAN_POINT ( 'NONE',  ( -170.0000000000000284, 14.99999999999999289, 0.000000000000000000 ) ) ;
#1886 = CARTESIAN_POINT ( 'NONE',  ( 13.21436662431716869, -4.623906867372263640, 26.57142857142857295 ) ) ;
#1887 = CARTESIAN_POINT ( 'NONE',  ( 14.26974319298268767, -1.607813917172876916, 32.35714285714286120 ) ) ;
#1888 = ORIENTED_EDGE ( 'NONE', *, *, #1274, .F. ) ;
#1889 = AXIS2_PLACEMENT_3D ( 'NONE', #1152, #1926, #9840 ) ;
#1890 = CARTESIAN_POINT ( 'NONE',  ( -16.30827793483735988, 1.837501619626141780, 47.35714285714286120 ) ) ;
#1891 = CARTESIAN_POINT ( 'NONE',  ( 2.000000000000001776, 1.329782007511007169, -0.7677500000000114788 ) ) ;
#1892 = CARTESIAN_POINT ( 'NONE',  ( -13.54758718765249625, -8.512513224245459753, 10.71428571428571708 ) ) ;
#1893 = FACE_OUTER_BOUND ( 'NONE', #8859, .T. ) ;
#1894 = CARTESIAN_POINT ( 'NONE',  ( 4.270415729527831772, 8.486213763410694000, 19.59886208192144963 ) ) ;
#1895 = CARTESIAN_POINT ( 'NONE',  ( 4.579542530753127672, -8.877401133907065756, 8.648862081921430800 ) ) ;
#1896 = CARTESIAN_POINT ( 'NONE',  ( 11.22385875690717683, -11.40355824106234373, 7.004040569626434731 ) ) ;
#1897 = CARTESIAN_POINT ( 'NONE',  ( -15.49051278174638036, -5.420364854932175902, 22.92857142857142705 ) ) ;
#1898 = FACE_OUTER_BOUND ( 'NONE', #1044, .T. ) ;
#1899 = CARTESIAN_POINT ( 'NONE',  ( 5.164528828830335705, -15.14410076328347543, 1.432611998197868219 ) ) ;
#1900 = CARTESIAN_POINT ( 'NONE',  ( -12.15899005565164792, 7.639999817571651697, 11.78571428571428115 ) ) ;
#1901 = DIRECTION ( 'NONE',  ( 1.000000000000000000, 0.000000000000000000, 0.000000000000000000 ) ) ;
#1902 = CARTESIAN_POINT ( 'NONE',  ( 5.056896391392317724, -9.814260835640970626, 11.64886208192146988 ) ) ;
#1903 = ORIENTED_EDGE ( 'NONE', *, *, #3, .T. ) ;
#1904 = CARTESIAN_POINT ( 'NONE',  ( -1.567502665446231180, -13.91197093850540334, 15.85714285714286120 ) ) ;
#1905 = ORIENTED_EDGE ( 'NONE', *, *, #6467, .T. ) ;
#1906 = CARTESIAN_POINT ( 'NONE',  ( -1.791431617652833763, -15.89939535829188877, 33.85714285714285410 ) ) ;
#1907 = CARTESIAN_POINT ( 'NONE',  ( 15.14410076328353227, -5.164528828830166063, 46.56738800180214355 ) ) ;
#1908 = CARTESIAN_POINT ( 'NONE',  ( 1.642561882922480621, -10.37072757624892638, 4.800000000000026468 ) ) ;
#1909 = EDGE_CURVE ( 'NONE', #6987, #5718, #9429, .T. ) ;
#1910 = CARTESIAN_POINT ( 'NONE',  ( -10.15407889436378852, -10.15407889436390398, 16.50000000000000000 ) ) ;
#1911 = CARTESIAN_POINT ( 'NONE',  ( 12.22833218042443271, -7.529642458189144349, 22.78167371608784464 ) ) ;
#1912 = ORIENTED_EDGE ( 'NONE', *, *, #4905, .F. ) ;
#1913 = SURFACE_SIDE_STYLE ('',( #7386 ) ) ;
#1914 = CARTESIAN_POINT ( 'NONE',  ( 55.99999999999996447, 0.000000000000000000, 0.000000000000000000 ) ) ;
#1915 = CARTESIAN_POINT ( 'NONE',  ( 4.619798703721856192, 13.59724543428036725, 39.06738800180213644 ) ) ;
#1916 = CARTESIAN_POINT ( 'NONE',  ( 9.814260835641038128, -5.056896391392198709, 12.35113791807855677 ) ) ;
#1917 = CARTESIAN_POINT ( 'NONE',  ( -4.809394265263009061, -9.333916720356716823, 7.101137918078564759 ) ) ;
#1918 = DIRECTION ( 'NONE',  ( -5.102127870520027391E-17, 1.000000000000000000, 0.000000000000000000 ) ) ;
#1919 = CARTESIAN_POINT ( 'NONE',  ( -12.08964793087886314, 7.750357176954159932, 15.78975485534072121 ) ) ;
#1920 = CARTESIAN_POINT ( 'NONE',  ( -4.503970704919988854, 13.25633410266674517, 28.43261199819786356 ) ) ;
#1921 = CARTESIAN_POINT ( 'NONE',  ( -1.727091770866549414, -10.90442828429185695, 4.950000000000017053 ) ) ;
#1922 = CARTESIAN_POINT ( 'NONE',  ( -1.665163862719845067, -15.91362231745477374, 35.85310228751641404 ) ) ;
#1923 = CARTESIAN_POINT ( 'NONE',  ( -8.870817433266022789, 13.12422867397192583, 48.72999999999998266 ) ) ;
#1924 = CARTESIAN_POINT ( 'NONE',  ( 15.10213328493390783, -5.284464991282587398, 20.57142857142857295 ) ) ;
#1925 = CARTESIAN_POINT ( 'NONE',  ( -5.297344310588352201, -15.53355953199867301, 6.067388001802139996 ) ) ;
#1926 = DIRECTION ( 'NONE',  ( -1.000000000000000000, -0.000000000000000000, -0.000000000000000000 ) ) ;
#1927 = CIRCLE ( 'NONE', #8535, 8.500000000000000000 ) ;
#1928 = CARTESIAN_POINT ( 'NONE',  ( -9.375578539472099848, 1.533232399700011461, 1.701137918078535094 ) ) ;
#1929 = CARTESIAN_POINT ( 'NONE',  ( 8.900167166472154889, -4.534861676072210912, 13.34999999999998188 ) ) ;
#1930 = DIRECTION ( 'NONE',  ( 0.000000000000000000, -8.191099868251446680E-34, -1.000000000000000000 ) ) ;
#1931 = CARTESIAN_POINT ( 'NONE',  ( -9.899494936611716867, 9.899494936611610285, 36.00000000000000711 ) ) ;
#1932 = EDGE_CURVE ( 'NONE', #2493, #4771, #5404, .T. ) ;
#1933 = AXIS2_PLACEMENT_3D ( 'NONE', #677, #4554, #5320 ) ;
#1934 = CARTESIAN_POINT ( 'NONE',  ( -14.26974319298268767, 1.607813917172874918, 35.35714285714285410 ) ) ;
#1935 = EDGE_LOOP ( 'NONE', ( #321, #4499, #6090, #10188 ) ) ;
#1936 = CARTESIAN_POINT ( 'NONE',  ( 1.665163862719847732, 15.91362231745477374, 2.853102287516426916 ) ) ;
#1937 = DIRECTION ( 'NONE',  ( -1.000000000000000000, 1.842239752758738928E-31, -1.780435181894459419E-32 ) ) ;
#1938 = CARTESIAN_POINT ( 'NONE',  ( 1.837501619626330074, -16.30827793483733501, 21.64285714285714590 ) ) ;
#1939 = DIRECTION ( 'NONE',  ( 0.000000000000000000, -6.338944243255235518E-49, 1.000000000000000000 ) ) ;
#1940 = CARTESIAN_POINT ( 'NONE',  ( -4.579542530753125895, 8.877401133907090625, 19.14886208192144679 ) ) ;
#1941 = CARTESIAN_POINT ( 'NONE',  ( 8.922933199037192509, -4.490180821391404287, 5.348862081921449629 ) ) ;
#1942 = CARTESIAN_POINT ( 'NONE',  ( 15.53355953199861794, 5.297344310588528060, 5.932611998197868886 ) ) ;
#1943 = CARTESIAN_POINT ( 'NONE',  ( -1.791431617652833763, -15.89939535829188877, 33.85714285714285410 ) ) ;
#1944 = EDGE_CURVE ( 'NONE', #2935, #8072, #7779, .T. ) ;
#1945 = CARTESIAN_POINT ( 'NONE',  ( -9.899494936611716867, 9.899494936611610285, 48.00000000000000000 ) ) ;
#1946 = CARTESIAN_POINT ( 'NONE',  ( -13.82664651025767100, 8.841785722321537477, 9.789754855340722983 ) ) ;
#1947 = CARTESIAN_POINT ( 'NONE',  ( 9.899494936611718643, -9.899494936611608509, 27.00000000000000355 ) ) ;
#1948 = CARTESIAN_POINT ( 'NONE',  ( -15.49051278174638036, -5.420364854932175902, 10.92857142857142883 ) ) ;
#1949 = CARTESIAN_POINT ( 'NONE',  ( 2.000000000000001776, -0.8865213383406761460, 1.535499999999911935 ) ) ;
#1950 = ORIENTED_EDGE ( 'NONE', *, *, #231, .F. ) ;
#1951 = CARTESIAN_POINT ( 'NONE',  ( 7.448449071214646722, 11.85413878919601594, 19.28571428571428825 ) ) ;
#1952 = VERTEX_POINT ( 'NONE', #3909 ) ;
#1953 = CARTESIAN_POINT ( 'NONE',  ( 8.512513224245308763, 13.54758718765259040, 25.28571428571428470 ) ) ;
#1954 = CARTESIAN_POINT ( 'NONE',  ( 8.841785722321695573, -13.82664651025757152, 47.21024514465928235 ) ) ;
#1955 = CARTESIAN_POINT ( 'NONE',  ( -10.37818827243067688, 1.595456901104525205, 3.698862081921452827 ) ) ;
#1956 = PRODUCT_DEFINITION_SHAPE ( 'NONE', 'NONE',  #4671 ) ;
#1957 = APPLICATION_PROTOCOL_DEFINITION ( 'draft international standard', 'automotive_design', 1998, #6570 ) ;
#1958 = CARTESIAN_POINT ( 'NONE',  ( -14.26974319298268767, 1.607813917172874696, 17.35714285714286120 ) ) ;
#1959 = ORIENTED_EDGE ( 'NONE', *, *, #1366, .F. ) ;
#1960 = CARTESIAN_POINT ( 'NONE',  ( 14.28433602490915000, -1.478298951650544479, 34.35310228751642825 ) ) ;
#1961 = EDGE_LOOP ( 'NONE', ( #9547, #8573, #8965, #2892, #5922 ) ) ;
#1962 = CARTESIAN_POINT ( 'NONE',  ( -4.246973736992222470, -14.10948682827616096, -1.270000000000007123 ) ) ;
#1963 = CARTESIAN_POINT ( 'NONE',  ( -4.579542530753125895, 8.877401133907083519, 4.148862081921444123 ) ) ;
#1964 = CARTESIAN_POINT ( 'NONE',  ( 7.806708723663831506, 7.806708723663931870, 3.749999999999997335 ) ) ;
#1965 = CARTESIAN_POINT ( 'NONE',  ( 7.390897758835871301, -7.458344646081617846, 6.501137918078588207 ) ) ;
#1966 = FACE_OUTER_BOUND ( 'NONE', #9024, .T. ) ;
#1967 = CARTESIAN_POINT ( 'NONE',  ( -1.478298951650703019, 14.28433602490913579, 22.64689771248357530 ) ) ;
#1968 = SHAPE_REPRESENTATION_RELATIONSHIP ( 'NONE' , 'NONE' ,  #1047, #2769 ) ;
#1969 = CARTESIAN_POINT ( 'NONE',  ( -14.25515036105622890, 1.737328882695209575, 27.36118342676929416 ) ) ;
#1970 = CARTESIAN_POINT ( 'NONE',  ( 1.642561882922480621, -10.37072757624892638, 4.800000000000026468 ) ) ;
#1971 = CARTESIAN_POINT ( 'NONE',  ( -15.44746603149413922, -5.543385399275820191, 42.92453085894499054 ) ) ;
#1972 = CARTESIAN_POINT ( 'NONE',  ( -13.10871455524824292, 7.195040570839012162, 48.73000000000001819 ) ) ;
#1973 = CARTESIAN_POINT ( 'NONE',  ( -11.31370849898482156, 11.31370849898469544, 24.00000000000000000 ) ) ;
#1974 = DIRECTION ( 'NONE',  ( 0.000000000000000000, 0.000000000000000000, 1.000000000000000000 ) ) ;
#1975 = CARTESIAN_POINT ( 'NONE',  ( 13.89774397934249706, 1.693770420379375308, 10.13881657323070762 ) ) ;
#1976 = CARTESIAN_POINT ( 'NONE',  ( -1.612135949262737844, -9.858066664633888365, 6.951137918078597266 ) ) ;
#1978 = COLOUR_RGB ( '', 0.66274510, 0.83137255, 0.94901961) ;
#1977 = CARTESIAN_POINT ( 'NONE',  ( -4.312909747525649706, -8.464561979789507973, 17.10000000000000497 ) ) ;
#1979 = CARTESIAN_POINT ( 'NONE',  ( -162.8500000000000512, -5.808233151972152598E-15, 15.00000000000000000 ) ) ;
#1980 = CARTESIAN_POINT ( 'NONE',  ( -13.21436662431716869, 4.623906867372262752, 29.57142857142857650 ) ) ;
#1981 = CARTESIAN_POINT ( 'NONE',  ( 1.567502665446232957, 13.91197093850540156, 36.85714285714286120 ) ) ;
#1982 = ORIENTED_EDGE ( 'NONE', *, *, #310, .T. ) ;
#1983 = VECTOR ( 'NONE', #3128, 1000.000000000000000 ) ;
#1984 = DIRECTION ( 'NONE',  ( -1.000000000000000000, -0.000000000000000000, -0.000000000000000000 ) ) ;
#1985 = CIRCLE ( 'NONE', #2326, 8.000000000000000000 ) ;
#1986 = CARTESIAN_POINT ( 'NONE',  ( 13.89598863503046111, -8.731428362939032795, 20.78571428571429180 ) ) ;
#1987 = DIRECTION ( 'NONE',  ( 1.000000000000000000, 4.755747939841215952E-17, -0.000000000000000000 ) ) ;
#1988 = DIRECTION ( 'NONE',  ( -4.575525868300071581E-16, -1.000000000000000000, 0.000000000000000000 ) ) ;
#1989 = SURFACE_STYLE_FILL_AREA ( #443 ) ;
#1990 = CARTESIAN_POINT ( 'NONE',  ( -7.027753727702738651, -7.098671581784262941, 18.24886208192143044 ) ) ;
#1991 = CARTESIAN_POINT ( 'NONE',  ( 8.442910196168311288, 4.355403765523574222, 4.898862081921403266 ) ) ;
#1992 = CARTESIAN_POINT ( 'NONE',  ( 11.69682198916835070, 11.51250119794901394, 5.504040569626439172 ) ) ;
#1993 = CIRCLE ( 'NONE', #8594, 2.000000000000001332 ) ;
#1994 = CARTESIAN_POINT ( 'NONE',  ( -15.89939535829186923, -1.791431617653016062, 29.14285714285714235 ) ) ;
#1995 = VECTOR ( 'NONE', #4731, 1000.000000000000000 ) ;
#1996 = AXIS2_PLACEMENT_3D ( 'NONE', #9059, #4397, #4242 ) ;
#1997 = EDGE_CURVE ( 'NONE', #5632, #3401, #5774, .T. ) ;
#1998 = CARTESIAN_POINT ( 'NONE',  ( -0.3021515714675195863, 13.99673906407701729, 48.73000000000003951 ) ) ;
#1999 = CARTESIAN_POINT ( 'NONE',  ( 15.91362231745475597, 1.665163862720026255, 12.14689771248358063 ) ) ;
#2000 = CARTESIAN_POINT ( 'NONE',  ( 4.742819248065503146, 13.55419868402813677, 25.07142857142858361 ) ) ;
#2001 = CARTESIAN_POINT ( 'NONE',  ( -158.0000000000000284, -13.00000000000001066, 1.592040838891559884E-15 ) ) ;
#2002 = CARTESIAN_POINT ( 'NONE',  ( 5.284464991282756152, -15.10213328493384743, 39.42857142857143060 ) ) ;
#2003 = VERTEX_POINT ( 'NONE', #3029 ) ;
#2004 = CARTESIAN_POINT ( 'NONE',  ( -13.55419868402807992, -4.742819248065651472, 16.92857142857143771 ) ) ;
#2005 = ORIENTED_EDGE ( 'NONE', *, *, #5772, .T. ) ;
#2006 = CARTESIAN_POINT ( 'NONE',  ( 13.54758718765249803, 8.512513224245457977, 37.71428571428571530 ) ) ;
#2007 = CARTESIAN_POINT ( 'NONE',  ( -14.28433602490915000, 1.478298951650542481, 7.353102287516419366 ) ) ;
#2008 = CARTESIAN_POINT ( 'NONE',  ( 4.724406229267374968, 9.377220287599055126, 1.598862081921434308 ) ) ;
#2009 = PRODUCT_CONTEXT ( 'NONE', #2233, 'mechanical' ) ;
#2010 = CARTESIAN_POINT ( 'NONE',  ( 7.448449071214646722, 11.85413878919601594, 13.28571428571429003 ) ) ;
#2011 = EDGE_CURVE ( 'NONE', #1692, #2905, #7742, .T. ) ;
#2012 = CARTESIAN_POINT ( 'NONE',  ( 4.619798703721856192, 13.59724543428036725, 27.06738800180213644 ) ) ;
#2013 = CARTESIAN_POINT ( 'NONE',  ( 10.37072757624895836, -1.642561882922355831, 19.19999999999999574 ) ) ;
#2014 = CARTESIAN_POINT ( 'NONE',  ( -166.5969417738770346, 0.4288646725500943613, 12.99335536005336955 ) ) ;
#2015 = CARTESIAN_POINT ( 'NONE',  ( 4.270415729527831772, 8.486213763410688671, 4.598862081921435419 ) ) ;
#2016 = CARTESIAN_POINT ( 'NONE',  ( 1.727091770866550968, 10.90442828429187294, 3.450000000000006839 ) ) ;
#2017 = CARTESIAN_POINT ( 'NONE',  ( -9.377220287598998283, -4.724406229267460233, 7.401137918078573463 ) ) ;
#2018 = CARTESIAN_POINT ( 'NONE',  ( -108.0000000000000284, 2.204364238465235428E-15, -18.00000000000000000 ) ) ;
#2019 = CARTESIAN_POINT ( 'NONE',  ( -11.92174236212692051, -7.340858601238089420, 26.71832628391215536 ) ) ;
#2020 = CARTESIAN_POINT ( 'NONE',  ( 1.727091770866550968, 10.90442828429186761, 6.449999999999969091 ) ) ;
#2021 = CARTESIAN_POINT ( 'NONE',  ( 11.51250119794888249, 11.69682198916847682, 45.49595943037356705 ) ) ;
#2022 = CARTESIAN_POINT ( 'NONE',  ( -1.642834855697749452, 15.92644139018836746, 48.73000000000002530 ) ) ;
#2023 = CARTESIAN_POINT ( 'NONE',  ( 0.000000000000000000, -6.162975822039154730E-30, 20.00000000000001776 ) ) ;
#2024 = CARTESIAN_POINT ( 'NONE',  ( 9.989344678689365153, -9.809645194533958446, 16.99595943037355994 ) ) ;
#2025 = CARTESIAN_POINT ( 'NONE',  ( -9.873755945037078874, -1.513077731353020594, 16.55113791807855605 ) ) ;
#2026 = CARTESIAN_POINT ( 'NONE',  ( -1.486127417882243895, 9.383039235653816590, 12.29999999999997762 ) ) ;
#2027 = CARTESIAN_POINT ( 'NONE',  ( 56.99999999999997158, 0.000000000000000000, 8.000000000000000000 ) ) ;
#2028 = CARTESIAN_POINT ( 'NONE',  ( -15.53355953199861794, -5.297344310588530725, 38.93261199819787777 ) ) ;
#2029 = CARTESIAN_POINT ( 'NONE',  ( 9.899494936611610285, 9.899494936611718643, 49.50000000000000711 ) ) ;
#2030 = CARTESIAN_POINT ( 'NONE',  ( 11.85413878919593422, 7.448449071214774619, 37.71428571428571530 ) ) ;
#2031 = ORIENTED_EDGE ( 'NONE', *, *, #3459, .F. ) ;
#2032 = CARTESIAN_POINT ( 'NONE',  ( 8.512513224245308763, 13.54758718765259040, 43.28571428571429180 ) ) ;
#2033 = DIRECTION ( 'NONE',  ( 0.000000000000000000, 0.000000000000000000, 1.000000000000000000 ) ) ;
#2034 = CARTESIAN_POINT ( 'NONE',  ( 11.31370849898482334, -11.31370849898469366, 33.00000000000000000 ) ) ;
#2035 = DIRECTION ( 'NONE',  ( -1.000000000000000000, -0.000000000000000000, -0.000000000000000000 ) ) ;
#2036 = DIRECTION ( 'NONE',  ( -1.000000000000000000, 0.000000000000000000, 0.000000000000000000 ) ) ;
#2037 = PRODUCT_DEFINITION_SHAPE ( 'NONE', 'NONE',  #4346 ) ;
#2038 = PLANE ( 'NONE',  #5285 ) ;
#2039 = CARTESIAN_POINT ( 'NONE',  ( 7.063212654743467489, 7.063212654743557195, 6.749999999999960032 ) ) ;
#2040 = CARTESIAN_POINT ( 'NONE',  ( -1.533232399700100057, 9.375578539472098072, 7.298862081921430267 ) ) ;
#2041 = UNCERTAINTY_MEASURE_WITH_UNIT (LENGTH_MEASURE( 1.000000000000000082E-05 ), #9661, 'distance_accuracy_value', 'NONE');
#2042 = CARTESIAN_POINT ( 'NONE',  ( 9.355568503977840678, 4.766900247265305701, 9.900000000000019895 ) ) ;
#2043 = CARTESIAN_POINT ( 'NONE',  ( -15.91362231745475597, -1.665163862720028254, 9.146897712483580634 ) ) ;
#2044 = CARTESIAN_POINT ( 'NONE',  ( 11.60466159355862104, 11.60466159355875071, 37.50000000000002842 ) ) ;
#2045 =( NAMED_UNIT ( * ) SI_UNIT ( $, .STERADIAN. ) SOLID_ANGLE_UNIT ( ) );
#2046 = AXIS2_PLACEMENT_3D ( 'NONE', #8898, #2536, #8744 ) ;
#2047 = CARTESIAN_POINT ( 'NONE',  ( 13.82664651025767100, -8.841785722321541030, 6.789754855340717654 ) ) ;
#2048 =( BOUNDED_SURFACE ( )  B_SPLINE_SURFACE ( 3, 2, ( 
 ( #6323, #9552, #9454, #6223, #5660, #7110, #4837, #130, #3282, #8038, #8716, #6271, #7885, #2311, #8619, #4688, #1590, #965, #811, #9504, #2409, #3079, #7163, #5457, #7989, #7835, #916, #2458, #5557, #6425, #1638, #9606, #8827, #4890, #2360, #1740, #4785, #6374, #5510, #4115, #5605, #3910, #10165, #7056, #10218, #8186, #7465, #1119, #289, #391, #1892, #9804, #8236, #1017, #4212, #2658, #9027, #4315, #4167, #5752, #1787, #5899, #3489, #3388, #7364, #3541, #9850, #5085, #8291, #2561, #1164, #8136, #9656, #7314, #6521, #6667, #6476, #3432, #9700, #6569, #8086, #5705, #8873, #9753, #5850, #5804, #2754, #237, #2608, #5143, #8920, #9075, #1837, #1212, #8981, #2708, #7261, #1986, #4992, #6619, #5040, #1938, #1071, #186, #3341, #4939, #4263, #7412, #340, #2908, #6768, #10105, #7623, #5953, #6826, #3799, #3635, #5289, #4576, #8446, #543, #7731, #9226, #6878, #5347, #8340, #1313, #10000, #6109, #1426, #1258, #2857, #9132, #3015, #597, #488, #4468, #650, #6935, #2199, #5392, #9899, #8500, #5235, #6715, #4417, #9953, #6159, #3583, #3692, #6002, #6051, #5192, #2806, #2034, #2142, #2960, #1372, #9336, #7566, #9181, #2245, #2087, #8551, #8390, #4363, #4524, #10048, #7516, #441, #7681, #3743, #9286, #7826, #1578, #118, #705, #5444, #4676, #7783, #1477, #3852, #3270, #3900, #6411, #905, #9385, #7044, #1528, #8753, #2445, #4726, #10153, #1681, #4824, #5591, #7872, #6210, #3174, #8605, #798, #852, #753, #6991, #7199, #5498, #68, #7977, #4052, #9588, #20, #10203, #9441, #3067, #2299, #3117, #6258, #2497, #2348, #8657, #3948, #4624, #9491, #7093, #3223, #6310, #6361, #2396, #5545, #9538, #8704, #1625, #4773 ),
 ( #5646, #7920, #4005, #7152, #4299, #6607, #953, #7301, #6558, #275, #9687, #3665, #6801, #8908, #2697, #4978, #9794, #1730, #1774, #1925, #5839, #3420, #2596, #8074, #3470, #2884, #5738, #519, #223, #7400, #9739, #8967, #3328, #4200, #8173, #1107, #5793, #7594, #9016, #1880, #4926, #8022, #1151, #6509, #8815, #4878, #5073, #1821, #2642, #6464, #4102, #5028, #8861, #7247, #4250, #8224, #9978, #8125, #168, #9643, #2549, #5693, #1001, #4152, #3376, #7352, #1058, #324, #9361, #6185, #6907, #627, #10179, #4555, #1402, #2273, #7807, #3095, #6855, #6235, #3044, #8635, #4703, #8527, #5371, #9412, #5259, #7653, #573, #2325, #7706, #4603, #3925, #7755, #7851, #5420, #678, #3775, #1453, #7020, #2993, #6966, #776, #5321, #8577, #730, #3828, #4654, #10076, #3878, #5475, #8477, #6136, #10128, #1557, #1501, #9312, #2117, #7070, #2225, #6396, #6027, #9207, #8418, #1347, #2179, #4501, #3718, #10027, #2937, #6079, #9257, #2373, #5524, #8683, #3145, #4755, #6286, #3980, #1605, #7130, #824, #7900, #9470, #3528, #2073, #1299, #7608, #5836, #3616, #5124, #1197, #5070, #8377, #5884, #4246, #8276, #5223, #1922, #6699, #2844, #9885, #9063, #5987, #7501, #5179, #6751, #6604, #9836, #4348, #4401, #9939, #9791, #1148, #7398, #4452, #9115, #9013, #2739, #528, #3678, #474, #6811, #8168, #2640, #6653, #5024, #2694, #8221, #5789, #1876, #1971, #4296, #425, #3467, #1104, #320, #2787, #1246, #5936, #8964, #7450, #377, #2021, #8328, #7550, #4563, #3936, #10089, #2283, #9988, #10189, #582, #8430, #7030, #6091, #3001, #8644, #9214, #3728, #2947, #6038, #2894, #2128, #1566, #2186, #4711, #9423, #7666, #5332, #10035, #3105, #739 ),
 ( #1462, #6863, #6145, #3887, #9268, #6244, #6975, #2335, #7860, #5380, #9323, #5486, #5269, #1356, #4511, #785, #8487, #8537, #1411, #4611, #7715, #9371, #7765, #636, #691, #3786, #6916, #3838, #10138, #3052, #5428, #1511, #6196, #8587, #4662, #7813, #4913, #9526, #893, #941, #8851, #8741, #3990, #1761, #1664, #2432, #155, #9675, #4863, #104, #8009, #3157, #1043, #5729, #988, #4041, #4086, #8060, #1809, #7289, #9480, #5578, #7236, #8799, #7962, #4965, #8115, #7187, #3362, #3257, #6497, #6296, #3212, #2383, #5532, #1718, #6398, #6348, #8691, #835, #9575, #4812, #2479, #5633, #3312, #6451, #9630, #2533, #3559, #6688, #1186, #2832, #9102, #7488, #312, #3409, #6736, #1911, #8363, #7338, #466, #5059, #9049, #1862, #262, #5108, #4232, #4188, #8263, #1236, #4388, #1138, #8317, #7539, #5011, #9153, #8949, #2012, #8158, #9825, #5166, #3606, #414, #4335, #8206, #9001, #9928, #2680, #9779, #9872, #5923, #7383, #5976, #2062, #5872, #4283, #3452, #5214, #6544, #7437, #9725, #5825, #2778, #2627, #5777, #1093, #2727, #6595, #363, #3512, #6641, #1960, #4598, #7650, #516, #3875, #9253, #5473, #4442, #7804, #2176, #6133, #9204, #7590, #2222, #1344, #1284, #5368, #8574, #1498, #8475, #5416, #4651, #2113, #6232, #6024, #9359, #5256, #6904, #2270, #727, #7752, #1450, #5318, #6076, #7017, #10024, #6852, #674, #3041, #10176, #8414, #3092, #8524, #9410, #2320, #3771, #624, #3662, #6798, #2881, #4498, #9974, #2934, #10072, #569, #2990, #3715, #3825, #9309, #1398, #6963, #4552, #7703, #10125, #6182, #7897, #929, #144, #7952, #7226, #7127, #3297, #6438, #822, #2422, #2469, #9621, #43, #5522, #2523, #3201, #3976 ),
 ( #6336, #4701, #4127, #5569, #5672, #8840, #1753, #6489, #7176, #4752, #9516, #773, #7066, #8214, #8731, #9667, #1652, #4799, #880, #1554, #4902, #4032, #93, #2575, #3248, #7276, #8001, #6386, #9565, #5620, #8050, #8789, #1706, #202, #4851, #4076, #979, #3354, #8632, #7848, #3922, #3139, #6283, #9467, #2370, #8681, #1603, #2620, #7479, #303, #8150, #9040, #8308, #3503, #8993, #6634, #5717, #9917, #4380, #9862, #2672, #9818, #6678, #1230, #3551, #8104, #4227, #2719, #7427, #6584, #456, #3597, #5818, #2767, #1904, #5916, #8886, #8937, #9089, #2004, #355, #9768, #5004, #408, #1799, #5053, #7531, #7376, #4328, #5863, #1951, #251, #1130, #5100, #8250, #1179, #6729, #5158, #4953, #1854, #1033, #4179, #3444, #7328, #3400, #6535, #8198, #9715, #5765, #1085, #4276, #6516, #436, #7407, #3536, #6662, #3427, #385, #9845, #4160, #1207, #1010, #4307, #7308, #1886, #7459, #2748, #9799, #6613, #7359, #1065, #5892, #4987, #1830, #2703, #8231, #9071, #230, #1980, #3481, #5137, #8285, #8976, #5800, #4358, #5700, #8080, #3383, #7511, #6471, #6564, #9649, #2556, #9694, #8867, #2603, #1781, #5745, #5035, #4934, #8914, #5845, #9023, #282, #4206, #8131, #9745, #2652, #1931, #1157, #8180, #1113, #4257, #5079, #333, #2241, #6047, #2902, #6927, #2798, #5186, #8335, #3794, #9176, #2137, #1470, #5280, #5386, #2955, #8441, #8385, #9221, #4571, #538, #4518, #8546, #2852, #6101, #5341, #1365, #2194, #2082, #8495, #1421, #5997, #7616, #7676, #7725, #5230, #483, #645, #1307, #4459, #6873, #6154, #592, #6821, #3737, #3576, #7776, #4619, #10100, #3687, #10043, #3010, #9330, #6709, #5947, #9995, #9280, #9893, #9127, #2029 ),
 ( #1253, #4411, #7560, #3625, #6762, #9947, #9534, #1574, #7195, #9582, #5641, #3894, #1674, #3166, #9487, #3113, #6406, #3943, #2294, #6304, #112, #10198, #1621, #900, #4769, #7087, #4048, #5540, #3219, #4820, #4670, #7866, #2391, #2441, #7970, #1523, #6253, #8809, #9432, #8748, #5493, #4872, #793, #6356, #700, #3265, #7821, #9380, #2490, #7038, #11, #1727, #10148, #748, #2341, #6985, #3847, #3061, #6205, #8651, #5437, #8598, #4721, #8700, #7915, #845, #4000, #7145, #63, #5585, #1145, #9008, #8123, #2544, #9735, #1769, #1053, #7393, #7296, #4097, #3523, #1817, #9788, #1919, #5067, #5882, #2636, #4147, #8903, #163, #6459, #5688, #4975, #5786, #8069, #4197, #7346, #949, #8960, #3322, #2690, #9638, #8216, #3461, #1872, #4291, #5020, #7448, #2735, #9060, #996, #373, #1100, #4243, #219, #1967, #8017, #8858, #7244, #4923, #3371, #6505, #2592, #2125, #8374, #5329, #9985, #7662, #6087, #9111, #5221, #526, #6861, #8485, #2019, #3614, #9881, #3782, #1354, #1244, #1295, #1409, #7713, #2944, #6143, #423, #4562, #5985, #7497, #5176, #4398, #634, #4344, #4450, #7547, #7601, #5933, #3566, #6696, #3674, #3725, #6808, #6914, #8326, #9164, #2891, #8272, #6033, #6745, #10084, #5265, #3000, #4508, #9319, #5117, #1194, #8881, #1026, #7323, #5564, #3349, #4846, #924, #4794, #8098, #5615, #3835, #7996, #1795, #1647, #3291, #2570, #6433, #8783, #5711, #7220, #4897, #6483, #6194, #9560, #4072, #4122, #9662, #9368, #875, #6973, #4173, #8835, #8726, #2465, #4947, #246, #197, #3395, #7761, #6530, #3243, #4610, #2280, #7947, #2232, #1460, #1701, #4027, #139, #3051, #686, #10135, #9616, #974, #2518, #5378, #7170 ),
 ( #8045, #8534, #88, #6381, #5667, #1748, #7270, #9813, #8351, #8931, #3439, #2666, #5760, #9709, #1848, #1269, #1899, #4428, #9141, #7371, #5048, #9763, #6724, #450, #2714, #8145, #9911, #2818, #3592, #5858, #4221, #1173, #6578, #9035, #9084, #8988, #4998, #5202, #3497, #8302, #5963, #2047, #7576, #8245, #5811, #7420, #1080, #298, #8193, #6627, #5095, #498, #6673, #3645, #2615, #1946, #4323, #1125, #4271, #350, #7473, #403, #3546, #9857, #2762, #5910, #1999, #5152, #1225, #4375, #7526, #7793, #3754, #7740, #8615, #6062, #9344, #8559, #6119, #5401, #5300, #1484, #4633, #9236, #606, #659, #712, #8457, #3702, #3861, #1382, #2152, #10113, #9395, #4586, #10058, #3808, #6782, #761, #5451, #7001, #6888, #6947, #10161, #2307, #3075, #9190, #4535, #3027, #8509, #7689, #1538, #4685, #2968, #9295, #9962, #6219, #2867, #10007, #7832, #6011, #1434, #2209, #5355, #2098, #5243, #6169, #8398, #2254, #1322, #4479, #7633, #553, #6834, #2917, #6420, #912, #2557, #8823, #7207, #28, #3125, #6472, #1634, #8081, #7053, #179, #4780, #8762, #1587, #10213, #4832, #3957, #3907, #7985, #961, #4111, #861, #8031, #7256, #4734, #8868, #8665, #1736, #7881, #9546, #4886, #3336, #126, #4061, #7931, #8712, #9650, #2405, #9499, #3278, #5654, #5701, #807, #1782, #4935, #9598, #2506, #4012, #7159, #6264, #5553, #77, #9451, #2356, #5507, #7101, #3182, #6317, #3230, #6368, #2454, #5599, #1691, #1011, #7309, #232, #1831, #3384, #2604, #4162, #4988, #6517, #9695, #5746, #8915, #10067, #1492, #7700, #1444, #2314, #10017, #3036, #2263, #2984, #9353, #9248, #5411, #8569, #2930, #4547, #4594, #4645, #2168, #7645, #7800, #5311, #6073 ),
 ( #9403, #722, #619, #8520, #3868, #6227, #7011, #2879, #8469, #7748, #2218, #1394, #5465, #8626, #3766, #6900, #3657, #10169, #6794, #3712, #3084, #1547, #5364, #6129, #9303, #4694, #511, #669, #9971, #3822, #6021, #6957, #10120, #5254, #6176, #9200, #2110, #8411, #1337, #4491, #565, #6847, #7060, #195, #5562, #1793, #767, #4121, #8723, #2463, #5516, #3914, #8781, #7891, #7841, #1699, #4895, #8043, #4790, #1746, #972, #8676, #2568, #2363, #5665, #1595, #3241, #816, #7267, #8833, #7944, #6278, #3347, #6481, #9660, #872, #4745, #9558, #3970, #4024, #7218, #7120, #10222, #5709, #1645, #6431, #8880, #3132, #9461, #6379, #36, #7168, #3193, #6329, #9510, #86, #5612, #2416, #4844, #7994, #922, #4070, #137, #9614, #3289, #2516, #4322, #1897, #3545, #5810, #1222, #3590, #9908, #8143, #5907, #7418, #3496, #7369, #448, #8191, #6527, #346, #4373, #4218, #5856, #5150, #9032, #1124, #8300, #9811, #7471, #9082, #8927, #5046, #6625, #6672, #1994, #1846, #3438, #9706, #6723, #1170, #1078, #4269, #7525, #2815, #2759, #5961, #244, #9140, #8986, #7321, #4997, #295, #4945, #4172, #2712, #6576, #1943, #5758, #3393, #2613, #5093, #9855, #8242, #8094, #9759, #2665, #1024, #400, #10112, #6833, #6217, #2150, #4583, #2044, #2253, #2865, #497, #5400, #8396, #5297, #711, #1267, #6010, #5242, #8350, #5200, #4426, #3858, #4475, #6999, #1483, #9961, #7632, #2206, #3806, #6167, #9189, #8557, #9294, #4631, #10160, #4532, #1381, #7791, #7575, #3642, #6780, #3073, #552, #604, #2094, #3751, #1321, #1432, #6886, #10006, #7688, #3025, #9234, #2967, #3699, #2915, #7739, #6943, #10057, #657, #6059, #8454, #6116, #5354, #8507 ) ),
 .UNSPECIFIED., .T., .F., .F. ) 
 B_SPLINE_SURFACE_WITH_KNOTS ( ( 4, 3, 4 ),
 ( 3, 2, 2, 2, 2, 2, 2, 2, 2, 2, 2, 2, 2, 2, 2, 2, 2, 2, 2, 2, 2, 2, 2, 2, 2, 2, 2, 2, 2, 2, 2, 2, 2, 2, 2, 2, 2, 2, 2, 2, 2, 2, 2, 2, 2, 2, 2, 2, 2, 2, 2, 2, 2, 2, 2, 2, 2, 2, 2, 2, 2, 2, 2, 2, 2, 2, 2, 2, 2, 2, 2, 2, 2, 2, 2, 2, 2, 2, 2, 2, 2, 2, 2, 2, 2, 2, 2, 2, 2, 2, 2, 2, 2, 2, 2, 2, 2, 2, 2, 2, 2, 2, 2, 2, 2, 2, 2, 2, 2, 2, 2, 2, 2, 2, 2, 2, 3 ),
 ( 0.000000000000000000, 0.5000000000000000000, 1.000000000000000000 ),
 ( 0.000000000000000000, 0.007936507936507936067, 0.01587301587301587213, 0.02380952380952380820, 0.03174603174603174427, 0.03968253968253968034, 0.04761904761904761640, 0.05555555555555555247, 0.06349206349206348854, 0.07142857142857142461, 0.07936507936507936067, 0.08730158730158729674, 0.09523809523809523281, 0.1031746031746031689, 0.1111111111111111049, 0.1190476190476190410, 0.1269841269841269771, 0.1349206349206349131, 0.1428571428571428492, 0.1507936507936507853, 0.1587301587301587213, 0.1666666666666666574, 0.1746031746031745935, 0.1825396825396825295, 0.1904761904761904656, 0.1984126984126984017, 0.2063492063492063378, 0.2142857142857142738, 0.2222222222222222099, 0.2301587301587301460, 0.2380952380952380820, 0.2460317460317460181, 0.2539682539682539542, 0.2619047619047619180, 0.2698412698412698263, 0.2777777777777777901, 0.2857142857142856984, 0.2936507936507936622, 0.3015873015873015706, 0.3095238095238095344, 0.3174603174603174427, 0.3253968253968254065, 0.3333333333333333148, 0.3412698412698412787, 0.3492063492063491870, 0.3571428571428571508, 0.3650793650793650591, 0.3730158730158730229, 0.3809523809523809312, 0.3888888888888888951, 0.3968253968253968034, 0.4047619047619047672, 0.4126984126984126755, 0.4206349206349206393, 0.4285714285714285476, 0.4365079365079365115, 0.4444444444444444198, 0.4523809523809523836, 0.4603174603174602919, 0.4682539682539682557, 0.4761904761904761640, 0.4841269841269841279, 0.4920634920634920362, 0.5000000000000000000, 0.5079365079365079083, 0.5158730158730159276, 0.5238095238095238360, 0.5317460317460317443, 0.5396825396825396526, 0.5476190476190476719, 0.5555555555555555802, 0.5634920634920634885, 0.5714285714285713969, 0.5793650793650794162, 0.5873015873015873245, 0.5952380952380952328, 0.6031746031746031411, 0.6111111111111111605, 0.6190476190476190688, 0.6269841269841269771, 0.6349206349206348854, 0.6428571428571429047, 0.6507936507936508130, 0.6587301587301587213, 0.6666666666666666297, 0.6746031746031746490, 0.6825396825396825573, 0.6904761904761904656, 0.6984126984126983739, 0.7063492063492063933, 0.7142857142857143016, 0.7222222222222222099, 0.7301587301587301182, 0.7380952380952381375, 0.7460317460317460458, 0.7539682539682539542, 0.7619047619047618625, 0.7698412698412698818, 0.7777777777777777901, 0.7857142857142856984, 0.7936507936507936067, 0.8015873015873016261, 0.8095238095238095344, 0.8174603174603174427, 0.8253968253968253510, 0.8333333333333333703, 0.8412698412698412787, 0.8492063492063491870, 0.8571428571428570953, 0.8650793650793651146, 0.8730158730158730229, 0.8809523809523809312, 0.8888888888888888395, 0.8968253968253968589, 0.9047619047619047672, 0.9126984126984126755, 0.9166666666666666297 ),
 .UNSPECIFIED. ) 
 GEOMETRIC_REPRESENTATION_ITEM ( )  RATIONAL_B_SPLINE_SURFACE ( (
 ( 1.000000000000000000, 0.9749279121818236193, 1.000000000000000000, 0.9749279121818236193, 1.000000000000000000, 0.9749279121818236193, 1.000000000000000000, 0.9749279121818236193, 1.000000000000000000, 0.9749279121818236193, 1.000000000000000000, 0.9749279121818236193, 1.000000000000000000, 0.9749279121818236193, 1.000000000000000000, 0.9749279121818236193, 1.000000000000000000, 0.9749279121818236193, 1.000000000000000000, 0.9749279121818236193, 1.000000000000000000, 0.9749279121818236193, 1.000000000000000000, 0.9749279121818236193, 1.000000000000000000, 0.9749279121818236193, 1.000000000000000000, 0.9749279121818236193, 1.000000000000000000, 0.9749279121818236193, 1.000000000000000000, 0.9749279121818236193, 1.000000000000000000, 0.9749279121818236193, 1.000000000000000000, 0.9749279121818236193, 1.000000000000000000, 0.9749279121818236193, 1.000000000000000000, 0.9749279121818236193, 1.000000000000000000, 0.9749279121818236193, 1.000000000000000000, 0.9749279121818236193, 1.000000000000000000, 0.9749279121818236193, 1.000000000000000000, 0.9749279121818236193, 1.000000000000000000, 0.9749279121818236193, 1.000000000000000000, 0.9749279121818236193, 1.000000000000000000, 0.9749279121818236193, 1.000000000000000000, 0.9749279121818236193, 1.000000000000000000, 0.9749279121818236193, 1.000000000000000000, 0.9749279121818236193, 1.000000000000000000, 0.9749279121818236193, 1.000000000000000000, 0.9749279121818236193, 1.000000000000000000, 0.9749279121818236193, 1.000000000000000000, 0.9749279121818236193, 1.000000000000000000, 0.9749279121818236193, 1.000000000000000000, 0.9749279121818236193, 1.000000000000000000, 0.9749279121818236193, 1.000000000000000000, 0.9749279121818236193, 1.000000000000000000, 0.9749279121818236193, 1.000000000000000000, 0.9749279121818236193, 1.000000000000000000, 0.9749279121818236193, 1.000000000000000000, 0.9749279121818236193, 1.000000000000000000, 0.9749279121818236193, 1.000000000000000000, 0.9749279121818236193, 1.000000000000000000, 0.9749279121818236193, 1.000000000000000000, 0.9749279121818236193, 1.000000000000000000, 0.9749279121818236193, 1.000000000000000000, 0.9749279121818236193, 1.000000000000000000, 0.9749279121818236193, 1.000000000000000000, 0.9749279121818236193, 1.000000000000000000, 0.9749279121818236193, 1.000000000000000000, 0.9749279121818236193, 1.000000000000000000, 0.9749279121818236193, 1.000000000000000000, 0.9749279121818236193, 1.000000000000000000, 0.9749279121818236193, 1.000000000000000000, 0.9749279121818236193, 1.000000000000000000, 0.9749279121818236193, 1.000000000000000000, 0.9749279121818236193, 1.000000000000000000, 0.9749279121818236193, 1.000000000000000000, 0.9749279121818236193, 1.000000000000000000, 0.9749279121818236193, 1.000000000000000000, 0.9749279121818236193, 1.000000000000000000, 0.9749279121818236193, 1.000000000000000000, 0.9749279121818236193, 1.000000000000000000, 0.9749279121818236193, 1.000000000000000000, 0.9749279121818236193, 1.000000000000000000, 0.9749279121818236193, 1.000000000000000000, 0.9749279121818236193, 1.000000000000000000, 0.9749279121818236193, 1.000000000000000000, 0.9749279121818236193, 1.000000000000000000, 0.9749279121818236193, 1.000000000000000000, 0.9749279121818236193, 1.000000000000000000, 0.9749279121818236193, 1.000000000000000000, 0.9749279121818236193, 1.000000000000000000, 0.9749279121818236193, 1.000000000000000000, 0.9749279121818236193, 1.000000000000000000, 0.9749279121818236193, 1.000000000000000000, 0.9749279121818236193, 1.000000000000000000, 0.9749279121818236193, 1.000000000000000000, 0.9749279121818236193, 1.000000000000000000, 0.9749279121818236193, 1.000000000000000000, 0.9749279121818236193, 1.000000000000000000, 0.9749279121818236193, 1.000000000000000000, 0.9749279121818236193, 1.000000000000000000, 0.9749279121818236193, 1.000000000000000000, 0.9749279121818236193, 1.000000000000000000, 0.9749279121818236193, 1.000000000000000000, 0.9749279121818236193, 1.000000000000000000, 0.9749279121818236193, 1.000000000000000000, 0.9749279121818236193, 1.000000000000000000, 0.9749279121818236193, 1.000000000000000000, 0.9749279121818236193, 1.000000000000000000, 0.9749279121818236193, 1.000000000000000000, 0.9749279121818236193, 1.000000000000000000, 0.9749279121818236193, 1.000000000000000000, 0.9749279121818236193, 1.000000000000000000, 0.9749279121818236193, 1.000000000000000000, 0.9749279121818236193, 1.000000000000000000, 0.9749279121818236193, 1.000000000000000000, 0.9749279121818236193, 1.000000000000000000, 0.9749279121818236193, 1.000000000000000000, 0.9749279121818236193, 1.000000000000000000, 0.9749279121818236193, 1.000000000000000000, 0.9749279121818236193, 1.000000000000000000, 0.9749279121818236193, 1.000000000000000000, 0.9749279121818236193, 1.000000000000000000, 0.9749279121818236193, 1.000000000000000000, 0.9749279121818236193, 1.000000000000000000, 0.9749279121818236193, 1.000000000000000000, 0.9749279121818236193, 1.000000000000000000, 0.9749279121818236193, 1.000000000000000000, 0.9749279121818236193, 1.000000000000000000, 0.9749279121818236193, 1.000000000000000000, 0.9749279121818236193, 1.000000000000000000, 0.9749279121818236193, 1.000000000000000000, 0.9874639560909117542, 0.9874639560909117542),
 ( 0.3333333333333333703, 0.3249759707272745768, 0.3333333333333333703, 0.3249759707272745768, 0.3333333333333333703, 0.3249759707272745768, 0.3333333333333333703, 0.3249759707272745768, 0.3333333333333333703, 0.3249759707272745768, 0.3333333333333333703, 0.3249759707272745768, 0.3333333333333333703, 0.3249759707272745768, 0.3333333333333333703, 0.3249759707272745768, 0.3333333333333333703, 0.3249759707272745768, 0.3333333333333333703, 0.3249759707272745768, 0.3333333333333333703, 0.3249759707272745768, 0.3333333333333333703, 0.3249759707272745768, 0.3333333333333333703, 0.3249759707272745768, 0.3333333333333333703, 0.3249759707272745768, 0.3333333333333333703, 0.3249759707272745768, 0.3333333333333333703, 0.3249759707272745768, 0.3333333333333333703, 0.3249759707272745768, 0.3333333333333333703, 0.3249759707272745768, 0.3333333333333333703, 0.3249759707272745768, 0.3333333333333333703, 0.3249759707272745768, 0.3333333333333333703, 0.3249759707272745768, 0.3333333333333333703, 0.3249759707272745768, 0.3333333333333333703, 0.3249759707272745768, 0.3333333333333333703, 0.3249759707272745768, 0.3333333333333333703, 0.3249759707272745768, 0.3333333333333333703, 0.3249759707272745768, 0.3333333333333333703, 0.3249759707272745768, 0.3333333333333333703, 0.3249759707272745768, 0.3333333333333333703, 0.3249759707272745768, 0.3333333333333333703, 0.3249759707272745768, 0.3333333333333333703, 0.3249759707272745768, 0.3333333333333333703, 0.3249759707272745768, 0.3333333333333333703, 0.3249759707272745768, 0.3333333333333333703, 0.3249759707272745768, 0.3333333333333333703, 0.3249759707272745768, 0.3333333333333333703, 0.3249759707272745768, 0.3333333333333333703, 0.3249759707272745768, 0.3333333333333333703, 0.3249759707272745768, 0.3333333333333333703, 0.3249759707272745768, 0.3333333333333333703, 0.3249759707272745768, 0.3333333333333333703, 0.3249759707272745768, 0.3333333333333333703, 0.3249759707272745768, 0.3333333333333333703, 0.3249759707272745768, 0.3333333333333333703, 0.3249759707272745768, 0.3333333333333333703, 0.3249759707272745768, 0.3333333333333333703, 0.3249759707272745768, 0.3333333333333333703, 0.3249759707272745768, 0.3333333333333333703, 0.3249759707272745768, 0.3333333333333333703, 0.3249759707272745768, 0.3333333333333333703, 0.3249759707272745768, 0.3333333333333333703, 0.3249759707272745768, 0.3333333333333333703, 0.3249759707272745768, 0.3333333333333333703, 0.3249759707272745768, 0.3333333333333333703, 0.3249759707272745768, 0.3333333333333333703, 0.3249759707272745768, 0.3333333333333333703, 0.3249759707272745768, 0.3333333333333333703, 0.3249759707272745768, 0.3333333333333333703, 0.3249759707272745768, 0.3333333333333333703, 0.3249759707272745768, 0.3333333333333333703, 0.3249759707272745768, 0.3333333333333333703, 0.3249759707272745768, 0.3333333333333333703, 0.3249759707272745768, 0.3333333333333333703, 0.3249759707272745768, 0.3333333333333333703, 0.3249759707272745768, 0.3333333333333333703, 0.3249759707272745768, 0.3333333333333333703, 0.3249759707272745768, 0.3333333333333333703, 0.3249759707272745768, 0.3333333333333333703, 0.3249759707272745768, 0.3333333333333333703, 0.3249759707272745768, 0.3333333333333333703, 0.3249759707272745768, 0.3333333333333333703, 0.3249759707272745768, 0.3333333333333333703, 0.3249759707272745768, 0.3333333333333333703, 0.3249759707272745768, 0.3333333333333333703, 0.3249759707272745768, 0.3333333333333333703, 0.3249759707272745768, 0.3333333333333333703, 0.3249759707272745768, 0.3333333333333333703, 0.3249759707272745768, 0.3333333333333333703, 0.3249759707272745768, 0.3333333333333333703, 0.3249759707272745768, 0.3333333333333333703, 0.3249759707272745768, 0.3333333333333333703, 0.3249759707272745768, 0.3333333333333333703, 0.3249759707272745768, 0.3333333333333333703, 0.3249759707272745768, 0.3333333333333333703, 0.3249759707272745768, 0.3333333333333333703, 0.3249759707272745768, 0.3333333333333333703, 0.3249759707272745768, 0.3333333333333333703, 0.3249759707272745768, 0.3333333333333333703, 0.3249759707272745768, 0.3333333333333333703, 0.3249759707272745768, 0.3333333333333333703, 0.3249759707272745768, 0.3333333333333333703, 0.3249759707272745768, 0.3333333333333333703, 0.3249759707272745768, 0.3333333333333333703, 0.3249759707272745768, 0.3333333333333333703, 0.3249759707272745768, 0.3333333333333333703, 0.3249759707272745768, 0.3333333333333333703, 0.3249759707272745768, 0.3333333333333333703, 0.3249759707272745768, 0.3333333333333333703, 0.3249759707272745768, 0.3333333333333333703, 0.3249759707272745768, 0.3333333333333333703, 0.3249759707272745768, 0.3333333333333333703, 0.3249759707272745768, 0.3333333333333333703, 0.3249759707272745768, 0.3333333333333333703, 0.3249759707272745768, 0.3333333333333333703, 0.3249759707272745768, 0.3333333333333333703, 0.3249759707272745768, 0.3333333333333333703, 0.3249759707272745768, 0.3333333333333333703, 0.3249759707272745768, 0.3333333333333333703, 0.3249759707272745768, 0.3333333333333333703, 0.3249759707272745768, 0.3333333333333333703, 0.3249759707272745768, 0.3333333333333333703, 0.3249759707272745768, 0.3333333333333333703, 0.3249759707272745768, 0.3333333333333333703, 0.3249759707272745768, 0.3333333333333333703, 0.3249759707272745768, 0.3333333333333333703, 0.3249759707272745768, 0.3333333333333333703, 0.3291546520303039736, 0.3291546520303039736),
 ( 0.3333333333333333703, 0.3249759707272745768, 0.3333333333333333703, 0.3249759707272745768, 0.3333333333333333703, 0.3249759707272745768, 0.3333333333333333703, 0.3249759707272745768, 0.3333333333333333703, 0.3249759707272745768, 0.3333333333333333703, 0.3249759707272745768, 0.3333333333333333703, 0.3249759707272745768, 0.3333333333333333703, 0.3249759707272745768, 0.3333333333333333703, 0.3249759707272745768, 0.3333333333333333703, 0.3249759707272745768, 0.3333333333333333703, 0.3249759707272745768, 0.3333333333333333703, 0.3249759707272745768, 0.3333333333333333703, 0.3249759707272745768, 0.3333333333333333703, 0.3249759707272745768, 0.3333333333333333703, 0.3249759707272745768, 0.3333333333333333703, 0.3249759707272745768, 0.3333333333333333703, 0.3249759707272745768, 0.3333333333333333703, 0.3249759707272745768, 0.3333333333333333703, 0.3249759707272745768, 0.3333333333333333703, 0.3249759707272745768, 0.3333333333333333703, 0.3249759707272745768, 0.3333333333333333703, 0.3249759707272745768, 0.3333333333333333703, 0.3249759707272745768, 0.3333333333333333703, 0.3249759707272745768, 0.3333333333333333703, 0.3249759707272745768, 0.3333333333333333703, 0.3249759707272745768, 0.3333333333333333703, 0.3249759707272745768, 0.3333333333333333703, 0.3249759707272745768, 0.3333333333333333703, 0.3249759707272745768, 0.3333333333333333703, 0.3249759707272745768, 0.3333333333333333703, 0.3249759707272745768, 0.3333333333333333703, 0.3249759707272745768, 0.3333333333333333703, 0.3249759707272745768, 0.3333333333333333703, 0.3249759707272745768, 0.3333333333333333703, 0.3249759707272745768, 0.3333333333333333703, 0.3249759707272745768, 0.3333333333333333703, 0.3249759707272745768, 0.3333333333333333703, 0.3249759707272745768, 0.3333333333333333703, 0.3249759707272745768, 0.3333333333333333703, 0.3249759707272745768, 0.3333333333333333703, 0.3249759707272745768, 0.3333333333333333703, 0.3249759707272745768, 0.3333333333333333703, 0.3249759707272745768, 0.3333333333333333703, 0.3249759707272745768, 0.3333333333333333703, 0.3249759707272745768, 0.3333333333333333703, 0.3249759707272745768, 0.3333333333333333703, 0.3249759707272745768, 0.3333333333333333703, 0.3249759707272745768, 0.3333333333333333703, 0.3249759707272745768, 0.3333333333333333703, 0.3249759707272745768, 0.3333333333333333703, 0.3249759707272745768, 0.3333333333333333703, 0.3249759707272745768, 0.3333333333333333703, 0.3249759707272745768, 0.3333333333333333703, 0.3249759707272745768, 0.3333333333333333703, 0.3249759707272745768, 0.3333333333333333703, 0.3249759707272745768, 0.3333333333333333703, 0.3249759707272745768, 0.3333333333333333703, 0.3249759707272745768, 0.3333333333333333703, 0.3249759707272745768, 0.3333333333333333703, 0.3249759707272745768, 0.3333333333333333703, 0.3249759707272745768, 0.3333333333333333703, 0.3249759707272745768, 0.3333333333333333703, 0.3249759707272745768, 0.3333333333333333703, 0.3249759707272745768, 0.3333333333333333703, 0.3249759707272745768, 0.3333333333333333703, 0.3249759707272745768, 0.3333333333333333703, 0.3249759707272745768, 0.3333333333333333703, 0.3249759707272745768, 0.3333333333333333703, 0.3249759707272745768, 0.3333333333333333703, 0.3249759707272745768, 0.3333333333333333703, 0.3249759707272745768, 0.3333333333333333703, 0.3249759707272745768, 0.3333333333333333703, 0.3249759707272745768, 0.3333333333333333703, 0.3249759707272745768, 0.3333333333333333703, 0.3249759707272745768, 0.3333333333333333703, 0.3249759707272745768, 0.3333333333333333703, 0.3249759707272745768, 0.3333333333333333703, 0.3249759707272745768, 0.3333333333333333703, 0.3249759707272745768, 0.3333333333333333703, 0.3249759707272745768, 0.3333333333333333703, 0.3249759707272745768, 0.3333333333333333703, 0.3249759707272745768, 0.3333333333333333703, 0.3249759707272745768, 0.3333333333333333703, 0.3249759707272745768, 0.3333333333333333703, 0.3249759707272745768, 0.3333333333333333703, 0.3249759707272745768, 0.3333333333333333703, 0.3249759707272745768, 0.3333333333333333703, 0.3249759707272745768, 0.3333333333333333703, 0.3249759707272745768, 0.3333333333333333703, 0.3249759707272745768, 0.3333333333333333703, 0.3249759707272745768, 0.3333333333333333703, 0.3249759707272745768, 0.3333333333333333703, 0.3249759707272745768, 0.3333333333333333703, 0.3249759707272745768, 0.3333333333333333703, 0.3249759707272745768, 0.3333333333333333703, 0.3249759707272745768, 0.3333333333333333703, 0.3249759707272745768, 0.3333333333333333703, 0.3249759707272745768, 0.3333333333333333703, 0.3249759707272745768, 0.3333333333333333703, 0.3249759707272745768, 0.3333333333333333703, 0.3249759707272745768, 0.3333333333333333703, 0.3249759707272745768, 0.3333333333333333703, 0.3249759707272745768, 0.3333333333333333703, 0.3249759707272745768, 0.3333333333333333703, 0.3249759707272745768, 0.3333333333333333703, 0.3249759707272745768, 0.3333333333333333703, 0.3249759707272745768, 0.3333333333333333703, 0.3249759707272745768, 0.3333333333333333703, 0.3249759707272745768, 0.3333333333333333703, 0.3249759707272745768, 0.3333333333333333703, 0.3249759707272745768, 0.3333333333333333703, 0.3249759707272745768, 0.3333333333333333703, 0.3249759707272745768, 0.3333333333333333703, 0.3249759707272745768, 0.3333333333333333703, 0.3249759707272745768, 0.3333333333333333703, 0.3291546520303039736, 0.3291546520303039736),
 ( 1.000000000000000000, 0.9749279121818236193, 1.000000000000000000, 0.9749279121818236193, 1.000000000000000000, 0.9749279121818236193, 1.000000000000000000, 0.9749279121818236193, 1.000000000000000000, 0.9749279121818236193, 1.000000000000000000, 0.9749279121818236193, 1.000000000000000000, 0.9749279121818236193, 1.000000000000000000, 0.9749279121818236193, 1.000000000000000000, 0.9749279121818236193, 1.000000000000000000, 0.9749279121818236193, 1.000000000000000000, 0.9749279121818236193, 1.000000000000000000, 0.9749279121818236193, 1.000000000000000000, 0.9749279121818236193, 1.000000000000000000, 0.9749279121818236193, 1.000000000000000000, 0.9749279121818236193, 1.000000000000000000, 0.9749279121818236193, 1.000000000000000000, 0.9749279121818236193, 1.000000000000000000, 0.9749279121818236193, 1.000000000000000000, 0.9749279121818236193, 1.000000000000000000, 0.9749279121818236193, 1.000000000000000000, 0.9749279121818236193, 1.000000000000000000, 0.9749279121818236193, 1.000000000000000000, 0.9749279121818236193, 1.000000000000000000, 0.9749279121818236193, 1.000000000000000000, 0.9749279121818236193, 1.000000000000000000, 0.9749279121818236193, 1.000000000000000000, 0.9749279121818236193, 1.000000000000000000, 0.9749279121818236193, 1.000000000000000000, 0.9749279121818236193, 1.000000000000000000, 0.9749279121818236193, 1.000000000000000000, 0.9749279121818236193, 1.000000000000000000, 0.9749279121818236193, 1.000000000000000000, 0.9749279121818236193, 1.000000000000000000, 0.9749279121818236193, 1.000000000000000000, 0.9749279121818236193, 1.000000000000000000, 0.9749279121818236193, 1.000000000000000000, 0.9749279121818236193, 1.000000000000000000, 0.9749279121818236193, 1.000000000000000000, 0.9749279121818236193, 1.000000000000000000, 0.9749279121818236193, 1.000000000000000000, 0.9749279121818236193, 1.000000000000000000, 0.9749279121818236193, 1.000000000000000000, 0.9749279121818236193, 1.000000000000000000, 0.9749279121818236193, 1.000000000000000000, 0.9749279121818236193, 1.000000000000000000, 0.9749279121818236193, 1.000000000000000000, 0.9749279121818236193, 1.000000000000000000, 0.9749279121818236193, 1.000000000000000000, 0.9749279121818236193, 1.000000000000000000, 0.9749279121818236193, 1.000000000000000000, 0.9749279121818236193, 1.000000000000000000, 0.9749279121818236193, 1.000000000000000000, 0.9749279121818236193, 1.000000000000000000, 0.9749279121818236193, 1.000000000000000000, 0.9749279121818236193, 1.000000000000000000, 0.9749279121818236193, 1.000000000000000000, 0.9749279121818236193, 1.000000000000000000, 0.9749279121818236193, 1.000000000000000000, 0.9749279121818236193, 1.000000000000000000, 0.9749279121818236193, 1.000000000000000000, 0.9749279121818236193, 1.000000000000000000, 0.9749279121818236193, 1.000000000000000000, 0.9749279121818236193, 1.000000000000000000, 0.9749279121818236193, 1.000000000000000000, 0.9749279121818236193, 1.000000000000000000, 0.9749279121818236193, 1.000000000000000000, 0.9749279121818236193, 1.000000000000000000, 0.9749279121818236193, 1.000000000000000000, 0.9749279121818236193, 1.000000000000000000, 0.9749279121818236193, 1.000000000000000000, 0.9749279121818236193, 1.000000000000000000, 0.9749279121818236193, 1.000000000000000000, 0.9749279121818236193, 1.000000000000000000, 0.9749279121818236193, 1.000000000000000000, 0.9749279121818236193, 1.000000000000000000, 0.9749279121818236193, 1.000000000000000000, 0.9749279121818236193, 1.000000000000000000, 0.9749279121818236193, 1.000000000000000000, 0.9749279121818236193, 1.000000000000000000, 0.9749279121818236193, 1.000000000000000000, 0.9749279121818236193, 1.000000000000000000, 0.9749279121818236193, 1.000000000000000000, 0.9749279121818236193, 1.000000000000000000, 0.9749279121818236193, 1.000000000000000000, 0.9749279121818236193, 1.000000000000000000, 0.9749279121818236193, 1.000000000000000000, 0.9749279121818236193, 1.000000000000000000, 0.9749279121818236193, 1.000000000000000000, 0.9749279121818236193, 1.000000000000000000, 0.9749279121818236193, 1.000000000000000000, 0.9749279121818236193, 1.000000000000000000, 0.9749279121818236193, 1.000000000000000000, 0.9749279121818236193, 1.000000000000000000, 0.9749279121818236193, 1.000000000000000000, 0.9749279121818236193, 1.000000000000000000, 0.9749279121818236193, 1.000000000000000000, 0.9749279121818236193, 1.000000000000000000, 0.9749279121818236193, 1.000000000000000000, 0.9749279121818236193, 1.000000000000000000, 0.9749279121818236193, 1.000000000000000000, 0.9749279121818236193, 1.000000000000000000, 0.9749279121818236193, 1.000000000000000000, 0.9749279121818236193, 1.000000000000000000, 0.9749279121818236193, 1.000000000000000000, 0.9749279121818236193, 1.000000000000000000, 0.9749279121818236193, 1.000000000000000000, 0.9749279121818236193, 1.000000000000000000, 0.9749279121818236193, 1.000000000000000000, 0.9749279121818236193, 1.000000000000000000, 0.9749279121818236193, 1.000000000000000000, 0.9749279121818236193, 1.000000000000000000, 0.9749279121818236193, 1.000000000000000000, 0.9749279121818236193, 1.000000000000000000, 0.9749279121818236193, 1.000000000000000000, 0.9749279121818236193, 1.000000000000000000, 0.9874639560909117542, 0.9874639560909117542),
 ( 0.3333333333333333703, 0.3249759707272745768, 0.3333333333333333703, 0.3249759707272745768, 0.3333333333333333703, 0.3249759707272745768, 0.3333333333333333703, 0.3249759707272745768, 0.3333333333333333703, 0.3249759707272745768, 0.3333333333333333703, 0.3249759707272745768, 0.3333333333333333703, 0.3249759707272745768, 0.3333333333333333703, 0.3249759707272745768, 0.3333333333333333703, 0.3249759707272745768, 0.3333333333333333703, 0.3249759707272745768, 0.3333333333333333703, 0.3249759707272745768, 0.3333333333333333703, 0.3249759707272745768, 0.3333333333333333703, 0.3249759707272745768, 0.3333333333333333703, 0.3249759707272745768, 0.3333333333333333703, 0.3249759707272745768, 0.3333333333333333703, 0.3249759707272745768, 0.3333333333333333703, 0.3249759707272745768, 0.3333333333333333703, 0.3249759707272745768, 0.3333333333333333703, 0.3249759707272745768, 0.3333333333333333703, 0.3249759707272745768, 0.3333333333333333703, 0.3249759707272745768, 0.3333333333333333703, 0.3249759707272745768, 0.3333333333333333703, 0.3249759707272745768, 0.3333333333333333703, 0.3249759707272745768, 0.3333333333333333703, 0.3249759707272745768, 0.3333333333333333703, 0.3249759707272745768, 0.3333333333333333703, 0.3249759707272745768, 0.3333333333333333703, 0.3249759707272745768, 0.3333333333333333703, 0.3249759707272745768, 0.3333333333333333703, 0.3249759707272745768, 0.3333333333333333703, 0.3249759707272745768, 0.3333333333333333703, 0.3249759707272745768, 0.3333333333333333703, 0.3249759707272745768, 0.3333333333333333703, 0.3249759707272745768, 0.3333333333333333703, 0.3249759707272745768, 0.3333333333333333703, 0.3249759707272745768, 0.3333333333333333703, 0.3249759707272745768, 0.3333333333333333703, 0.3249759707272745768, 0.3333333333333333703, 0.3249759707272745768, 0.3333333333333333703, 0.3249759707272745768, 0.3333333333333333703, 0.3249759707272745768, 0.3333333333333333703, 0.3249759707272745768, 0.3333333333333333703, 0.3249759707272745768, 0.3333333333333333703, 0.3249759707272745768, 0.3333333333333333703, 0.3249759707272745768, 0.3333333333333333703, 0.3249759707272745768, 0.3333333333333333703, 0.3249759707272745768, 0.3333333333333333703, 0.3249759707272745768, 0.3333333333333333703, 0.3249759707272745768, 0.3333333333333333703, 0.3249759707272745768, 0.3333333333333333703, 0.3249759707272745768, 0.3333333333333333703, 0.3249759707272745768, 0.3333333333333333703, 0.3249759707272745768, 0.3333333333333333703, 0.3249759707272745768, 0.3333333333333333703, 0.3249759707272745768, 0.3333333333333333703, 0.3249759707272745768, 0.3333333333333333703, 0.3249759707272745768, 0.3333333333333333703, 0.3249759707272745768, 0.3333333333333333703, 0.3249759707272745768, 0.3333333333333333703, 0.3249759707272745768, 0.3333333333333333703, 0.3249759707272745768, 0.3333333333333333703, 0.3249759707272745768, 0.3333333333333333703, 0.3249759707272745768, 0.3333333333333333703, 0.3249759707272745768, 0.3333333333333333703, 0.3249759707272745768, 0.3333333333333333703, 0.3249759707272745768, 0.3333333333333333703, 0.3249759707272745768, 0.3333333333333333703, 0.3249759707272745768, 0.3333333333333333703, 0.3249759707272745768, 0.3333333333333333703, 0.3249759707272745768, 0.3333333333333333703, 0.3249759707272745768, 0.3333333333333333703, 0.3249759707272745768, 0.3333333333333333703, 0.3249759707272745768, 0.3333333333333333703, 0.3249759707272745768, 0.3333333333333333703, 0.3249759707272745768, 0.3333333333333333703, 0.3249759707272745768, 0.3333333333333333703, 0.3249759707272745768, 0.3333333333333333703, 0.3249759707272745768, 0.3333333333333333703, 0.3249759707272745768, 0.3333333333333333703, 0.3249759707272745768, 0.3333333333333333703, 0.3249759707272745768, 0.3333333333333333703, 0.3249759707272745768, 0.3333333333333333703, 0.3249759707272745768, 0.3333333333333333703, 0.3249759707272745768, 0.3333333333333333703, 0.3249759707272745768, 0.3333333333333333703, 0.3249759707272745768, 0.3333333333333333703, 0.3249759707272745768, 0.3333333333333333703, 0.3249759707272745768, 0.3333333333333333703, 0.3249759707272745768, 0.3333333333333333703, 0.3249759707272745768, 0.3333333333333333703, 0.3249759707272745768, 0.3333333333333333703, 0.3249759707272745768, 0.3333333333333333703, 0.3249759707272745768, 0.3333333333333333703, 0.3249759707272745768, 0.3333333333333333703, 0.3249759707272745768, 0.3333333333333333703, 0.3249759707272745768, 0.3333333333333333703, 0.3249759707272745768, 0.3333333333333333703, 0.3249759707272745768, 0.3333333333333333703, 0.3249759707272745768, 0.3333333333333333703, 0.3249759707272745768, 0.3333333333333333703, 0.3249759707272745768, 0.3333333333333333703, 0.3249759707272745768, 0.3333333333333333703, 0.3249759707272745768, 0.3333333333333333703, 0.3249759707272745768, 0.3333333333333333703, 0.3249759707272745768, 0.3333333333333333703, 0.3249759707272745768, 0.3333333333333333703, 0.3249759707272745768, 0.3333333333333333703, 0.3249759707272745768, 0.3333333333333333703, 0.3249759707272745768, 0.3333333333333333703, 0.3249759707272745768, 0.3333333333333333703, 0.3249759707272745768, 0.3333333333333333703, 0.3249759707272745768, 0.3333333333333333703, 0.3249759707272745768, 0.3333333333333333703, 0.3249759707272745768, 0.3333333333333333703, 0.3249759707272745768, 0.3333333333333333703, 0.3291546520303039736, 0.3291546520303039736),
 ( 0.3333333333333333703, 0.3249759707272745768, 0.3333333333333333703, 0.3249759707272745768, 0.3333333333333333703, 0.3249759707272745768, 0.3333333333333333703, 0.3249759707272745768, 0.3333333333333333703, 0.3249759707272745768, 0.3333333333333333703, 0.3249759707272745768, 0.3333333333333333703, 0.3249759707272745768, 0.3333333333333333703, 0.3249759707272745768, 0.3333333333333333703, 0.3249759707272745768, 0.3333333333333333703, 0.3249759707272745768, 0.3333333333333333703, 0.3249759707272745768, 0.3333333333333333703, 0.3249759707272745768, 0.3333333333333333703, 0.3249759707272745768, 0.3333333333333333703, 0.3249759707272745768, 0.3333333333333333703, 0.3249759707272745768, 0.3333333333333333703, 0.3249759707272745768, 0.3333333333333333703, 0.3249759707272745768, 0.3333333333333333703, 0.3249759707272745768, 0.3333333333333333703, 0.3249759707272745768, 0.3333333333333333703, 0.3249759707272745768, 0.3333333333333333703, 0.3249759707272745768, 0.3333333333333333703, 0.3249759707272745768, 0.3333333333333333703, 0.3249759707272745768, 0.3333333333333333703, 0.3249759707272745768, 0.3333333333333333703, 0.3249759707272745768, 0.3333333333333333703, 0.3249759707272745768, 0.3333333333333333703, 0.3249759707272745768, 0.3333333333333333703, 0.3249759707272745768, 0.3333333333333333703, 0.3249759707272745768, 0.3333333333333333703, 0.3249759707272745768, 0.3333333333333333703, 0.3249759707272745768, 0.3333333333333333703, 0.3249759707272745768, 0.3333333333333333703, 0.3249759707272745768, 0.3333333333333333703, 0.3249759707272745768, 0.3333333333333333703, 0.3249759707272745768, 0.3333333333333333703, 0.3249759707272745768, 0.3333333333333333703, 0.3249759707272745768, 0.3333333333333333703, 0.3249759707272745768, 0.3333333333333333703, 0.3249759707272745768, 0.3333333333333333703, 0.3249759707272745768, 0.3333333333333333703, 0.3249759707272745768, 0.3333333333333333703, 0.3249759707272745768, 0.3333333333333333703, 0.3249759707272745768, 0.3333333333333333703, 0.3249759707272745768, 0.3333333333333333703, 0.3249759707272745768, 0.3333333333333333703, 0.3249759707272745768, 0.3333333333333333703, 0.3249759707272745768, 0.3333333333333333703, 0.3249759707272745768, 0.3333333333333333703, 0.3249759707272745768, 0.3333333333333333703, 0.3249759707272745768, 0.3333333333333333703, 0.3249759707272745768, 0.3333333333333333703, 0.3249759707272745768, 0.3333333333333333703, 0.3249759707272745768, 0.3333333333333333703, 0.3249759707272745768, 0.3333333333333333703, 0.3249759707272745768, 0.3333333333333333703, 0.3249759707272745768, 0.3333333333333333703, 0.3249759707272745768, 0.3333333333333333703, 0.3249759707272745768, 0.3333333333333333703, 0.3249759707272745768, 0.3333333333333333703, 0.3249759707272745768, 0.3333333333333333703, 0.3249759707272745768, 0.3333333333333333703, 0.3249759707272745768, 0.3333333333333333703, 0.3249759707272745768, 0.3333333333333333703, 0.3249759707272745768, 0.3333333333333333703, 0.3249759707272745768, 0.3333333333333333703, 0.3249759707272745768, 0.3333333333333333703, 0.3249759707272745768, 0.3333333333333333703, 0.3249759707272745768, 0.3333333333333333703, 0.3249759707272745768, 0.3333333333333333703, 0.3249759707272745768, 0.3333333333333333703, 0.3249759707272745768, 0.3333333333333333703, 0.3249759707272745768, 0.3333333333333333703, 0.3249759707272745768, 0.3333333333333333703, 0.3249759707272745768, 0.3333333333333333703, 0.3249759707272745768, 0.3333333333333333703, 0.3249759707272745768, 0.3333333333333333703, 0.3249759707272745768, 0.3333333333333333703, 0.3249759707272745768, 0.3333333333333333703, 0.3249759707272745768, 0.3333333333333333703, 0.3249759707272745768, 0.3333333333333333703, 0.3249759707272745768, 0.3333333333333333703, 0.3249759707272745768, 0.3333333333333333703, 0.3249759707272745768, 0.3333333333333333703, 0.3249759707272745768, 0.3333333333333333703, 0.3249759707272745768, 0.3333333333333333703, 0.3249759707272745768, 0.3333333333333333703, 0.3249759707272745768, 0.3333333333333333703, 0.3249759707272745768, 0.3333333333333333703, 0.3249759707272745768, 0.3333333333333333703, 0.3249759707272745768, 0.3333333333333333703, 0.3249759707272745768, 0.3333333333333333703, 0.3249759707272745768, 0.3333333333333333703, 0.3249759707272745768, 0.3333333333333333703, 0.3249759707272745768, 0.3333333333333333703, 0.3249759707272745768, 0.3333333333333333703, 0.3249759707272745768, 0.3333333333333333703, 0.3249759707272745768, 0.3333333333333333703, 0.3249759707272745768, 0.3333333333333333703, 0.3249759707272745768, 0.3333333333333333703, 0.3249759707272745768, 0.3333333333333333703, 0.3249759707272745768, 0.3333333333333333703, 0.3249759707272745768, 0.3333333333333333703, 0.3249759707272745768, 0.3333333333333333703, 0.3249759707272745768, 0.3333333333333333703, 0.3249759707272745768, 0.3333333333333333703, 0.3249759707272745768, 0.3333333333333333703, 0.3249759707272745768, 0.3333333333333333703, 0.3249759707272745768, 0.3333333333333333703, 0.3249759707272745768, 0.3333333333333333703, 0.3249759707272745768, 0.3333333333333333703, 0.3249759707272745768, 0.3333333333333333703, 0.3249759707272745768, 0.3333333333333333703, 0.3249759707272745768, 0.3333333333333333703, 0.3249759707272745768, 0.3333333333333333703, 0.3249759707272745768, 0.3333333333333333703, 0.3291546520303039736, 0.3291546520303039736),
 ( 1.000000000000000000, 0.9749279121818236193, 1.000000000000000000, 0.9749279121818236193, 1.000000000000000000, 0.9749279121818236193, 1.000000000000000000, 0.9749279121818236193, 1.000000000000000000, 0.9749279121818236193, 1.000000000000000000, 0.9749279121818236193, 1.000000000000000000, 0.9749279121818236193, 1.000000000000000000, 0.9749279121818236193, 1.000000000000000000, 0.9749279121818236193, 1.000000000000000000, 0.9749279121818236193, 1.000000000000000000, 0.9749279121818236193, 1.000000000000000000, 0.9749279121818236193, 1.000000000000000000, 0.9749279121818236193, 1.000000000000000000, 0.9749279121818236193, 1.000000000000000000, 0.9749279121818236193, 1.000000000000000000, 0.9749279121818236193, 1.000000000000000000, 0.9749279121818236193, 1.000000000000000000, 0.9749279121818236193, 1.000000000000000000, 0.9749279121818236193, 1.000000000000000000, 0.9749279121818236193, 1.000000000000000000, 0.9749279121818236193, 1.000000000000000000, 0.9749279121818236193, 1.000000000000000000, 0.9749279121818236193, 1.000000000000000000, 0.9749279121818236193, 1.000000000000000000, 0.9749279121818236193, 1.000000000000000000, 0.9749279121818236193, 1.000000000000000000, 0.9749279121818236193, 1.000000000000000000, 0.9749279121818236193, 1.000000000000000000, 0.9749279121818236193, 1.000000000000000000, 0.9749279121818236193, 1.000000000000000000, 0.9749279121818236193, 1.000000000000000000, 0.9749279121818236193, 1.000000000000000000, 0.9749279121818236193, 1.000000000000000000, 0.9749279121818236193, 1.000000000000000000, 0.9749279121818236193, 1.000000000000000000, 0.9749279121818236193, 1.000000000000000000, 0.9749279121818236193, 1.000000000000000000, 0.9749279121818236193, 1.000000000000000000, 0.9749279121818236193, 1.000000000000000000, 0.9749279121818236193, 1.000000000000000000, 0.9749279121818236193, 1.000000000000000000, 0.9749279121818236193, 1.000000000000000000, 0.9749279121818236193, 1.000000000000000000, 0.9749279121818236193, 1.000000000000000000, 0.9749279121818236193, 1.000000000000000000, 0.9749279121818236193, 1.000000000000000000, 0.9749279121818236193, 1.000000000000000000, 0.9749279121818236193, 1.000000000000000000, 0.9749279121818236193, 1.000000000000000000, 0.9749279121818236193, 1.000000000000000000, 0.9749279121818236193, 1.000000000000000000, 0.9749279121818236193, 1.000000000000000000, 0.9749279121818236193, 1.000000000000000000, 0.9749279121818236193, 1.000000000000000000, 0.9749279121818236193, 1.000000000000000000, 0.9749279121818236193, 1.000000000000000000, 0.9749279121818236193, 1.000000000000000000, 0.9749279121818236193, 1.000000000000000000, 0.9749279121818236193, 1.000000000000000000, 0.9749279121818236193, 1.000000000000000000, 0.9749279121818236193, 1.000000000000000000, 0.9749279121818236193, 1.000000000000000000, 0.9749279121818236193, 1.000000000000000000, 0.9749279121818236193, 1.000000000000000000, 0.9749279121818236193, 1.000000000000000000, 0.9749279121818236193, 1.000000000000000000, 0.9749279121818236193, 1.000000000000000000, 0.9749279121818236193, 1.000000000000000000, 0.9749279121818236193, 1.000000000000000000, 0.9749279121818236193, 1.000000000000000000, 0.9749279121818236193, 1.000000000000000000, 0.9749279121818236193, 1.000000000000000000, 0.9749279121818236193, 1.000000000000000000, 0.9749279121818236193, 1.000000000000000000, 0.9749279121818236193, 1.000000000000000000, 0.9749279121818236193, 1.000000000000000000, 0.9749279121818236193, 1.000000000000000000, 0.9749279121818236193, 1.000000000000000000, 0.9749279121818236193, 1.000000000000000000, 0.9749279121818236193, 1.000000000000000000, 0.9749279121818236193, 1.000000000000000000, 0.9749279121818236193, 1.000000000000000000, 0.9749279121818236193, 1.000000000000000000, 0.9749279121818236193, 1.000000000000000000, 0.9749279121818236193, 1.000000000000000000, 0.9749279121818236193, 1.000000000000000000, 0.9749279121818236193, 1.000000000000000000, 0.9749279121818236193, 1.000000000000000000, 0.9749279121818236193, 1.000000000000000000, 0.9749279121818236193, 1.000000000000000000, 0.9749279121818236193, 1.000000000000000000, 0.9749279121818236193, 1.000000000000000000, 0.9749279121818236193, 1.000000000000000000, 0.9749279121818236193, 1.000000000000000000, 0.9749279121818236193, 1.000000000000000000, 0.9749279121818236193, 1.000000000000000000, 0.9749279121818236193, 1.000000000000000000, 0.9749279121818236193, 1.000000000000000000, 0.9749279121818236193, 1.000000000000000000, 0.9749279121818236193, 1.000000000000000000, 0.9749279121818236193, 1.000000000000000000, 0.9749279121818236193, 1.000000000000000000, 0.9749279121818236193, 1.000000000000000000, 0.9749279121818236193, 1.000000000000000000, 0.9749279121818236193, 1.000000000000000000, 0.9749279121818236193, 1.000000000000000000, 0.9749279121818236193, 1.000000000000000000, 0.9749279121818236193, 1.000000000000000000, 0.9749279121818236193, 1.000000000000000000, 0.9749279121818236193, 1.000000000000000000, 0.9749279121818236193, 1.000000000000000000, 0.9749279121818236193, 1.000000000000000000, 0.9749279121818236193, 1.000000000000000000, 0.9749279121818236193, 1.000000000000000000, 0.9749279121818236193, 1.000000000000000000, 0.9874639560909117542, 0.9874639560909117542) ) ) 
 REPRESENTATION_ITEM ( '' )  SURFACE ( )  );
#2049 = CARTESIAN_POINT ( 'NONE',  ( 10.15407889436379030, 10.15407889436390576, 19.50000000000000355 ) ) ;
#2050 = CARTESIAN_POINT ( 'NONE',  ( 5.284464991282756152, -15.10213328493384743, 3.428571428571426605 ) ) ;
#2051 = CARTESIAN_POINT ( 'NONE',  ( 15.10213328493390783, -5.284464991282587398, 44.57142857142857650 ) ) ;
#2052 = ORIENTED_EDGE ( 'NONE', *, *, #161, .F. ) ;
#2053 = CARTESIAN_POINT ( 'NONE',  ( -10.37072757624895836, 1.642561882922380923, 17.69999999999999218 ) ) ;
#2054 = ORIENTED_EDGE ( 'NONE', *, *, #3567, .F. ) ;
#2055 = CARTESIAN_POINT ( 'NONE',  ( -8.731428362939187338, 13.89598863503036164, 30.21428571428572241 ) ) ;
#2056 = CARTESIAN_POINT ( 'NONE',  ( 11.22385875690704715, 11.40355824106246985, 51.49595943037355994 ) ) ;
#2057 = CARTESIAN_POINT ( 'NONE',  ( -5.056896391392315948, 9.814260835640991942, 4.148862081921444123 ) ) ;
#2058 = PRODUCT_CONTEXT ( 'NONE', #2562, 'mechanical' ) ;
#2059 = CARTESIAN_POINT ( 'NONE',  ( 9.899494936611718643, -9.899494936611608509, 21.00000000000000355 ) ) ;
#2060 = EDGE_CURVE ( 'NONE', #6536, #503, #1004, .T. ) ;
#2061 = EDGE_LOOP ( 'NONE', ( #252, #784, #3897, #9819 ) ) ;
#2062 = CARTESIAN_POINT ( 'NONE',  ( -10.06191849875405531, -10.24623928997363542, 30.49595943037356349 ) ) ;
#2063 = ORIENTED_EDGE ( 'NONE', *, *, #3301, .F. ) ;
#2064 = PRESENTATION_STYLE_ASSIGNMENT (( #4390 ) ) ;
#2065 = CARTESIAN_POINT ( 'NONE',  ( -170.0000000000000284, 11.00000000000000178, 1.469576158976824539E-15 ) ) ;
#2066 = CARTESIAN_POINT ( 'NONE',  ( 8.922933199037192509, -4.490180821391407839, 2.348862081921457623 ) ) ;
#2067 = CARTESIAN_POINT ( 'NONE',  ( -4.742819248065502258, -13.55419868402813677, 4.071428571428569398 ) ) ;
#2068 = CARTESIAN_POINT ( 'NONE',  ( -9.837026868206066865, 5.012215536711413399, 2.849999999999968114 ) ) ;
#2069 = CARTESIAN_POINT ( 'NONE',  ( 10.36326688006723984, -1.689666864740212215, 15.20113791807854575 ) ) ;
#2070 = PLANE ( 'NONE',  #7115 ) ;
#2071 = EDGE_LOOP ( 'NONE', ( #9101, #6799, #2031, #8766 ) ) ;
#2072 = CARTESIAN_POINT ( 'NONE',  ( -7.424621202458789426, 7.424621202458724589, 6.000000000000005329 ) ) ;
#2073 = CARTESIAN_POINT ( 'NONE',  ( 5.297344310588354865, 15.53355953199867301, 33.06738800180213644 ) ) ;
#2074 = EDGE_LOOP ( 'NONE', ( #5257, #2621, #7678, #7409 ) ) ;
#2075 = CARTESIAN_POINT ( 'NONE',  ( -12.99366168247997955, 7.244709680106955041, 48.73000000000001819 ) ) ;
#2076 = CARTESIAN_POINT ( 'NONE',  ( 15.49051278174638036, 5.420364854932175014, 31.92857142857143415 ) ) ;
#2077 = CARTESIAN_POINT ( 'NONE',  ( -58.00000000000002842, 2.079464148194916361E-15, -18.00000000000002132 ) ) ;
#2078 = CARTESIAN_POINT ( 'NONE',  ( -1.737328882695368115, 14.25515036105620581, 14.63881657323070939 ) ) ;
#2079 = CARTESIAN_POINT ( 'NONE',  ( 4.355403765523470305, 8.442910196168364578, 11.60113791807856742 ) ) ;
#2080 = CARTESIAN_POINT ( 'NONE',  ( -6.683790977649319842, 6.751237864895101026, 5.001137918078545574 ) ) ;
#2081 = CARTESIAN_POINT ( 'NONE',  ( -164.0471552234704689, 1.932476761857848668, 14.87509648533473516 ) ) ;
#2082 = CARTESIAN_POINT ( 'NONE',  ( 4.742819248065503146, 13.55419868402813677, 43.07142857142858361 ) ) ;
#2083 = CARTESIAN_POINT ( 'NONE',  ( -11.85413878919593422, -7.448449071214776396, 34.71428571428571530 ) ) ;
#2084 = EDGE_LOOP ( 'NONE', ( #7589, #5189 ) ) ;
#2085 = CARTESIAN_POINT ( 'NONE',  ( -15.10213328493390961, 5.284464991282586510, 41.57142857142856940 ) ) ;
#2086 = CARTESIAN_POINT ( 'NONE',  ( -68.00000000000002842, 1.004210375300829674E-15, -8.200000000000001066 ) ) ;
#2087 = CARTESIAN_POINT ( 'NONE',  ( -13.54758718765249625, -8.512513224245459753, 34.71428571428571530 ) ) ;
#2088 = CARTESIAN_POINT ( 'NONE',  ( 0.000000000000000000, -1.773042676681352292, -1.110223024625156540E-13 ) ) ;
#2089 = CARTESIAN_POINT ( 'NONE',  ( -9.837026868206066865, 5.012215536711413399, 2.849999999999968114 ) ) ;
#2090 = CARTESIAN_POINT ( 'NONE',  ( -8.900167166472156666, 4.534861676072234893, 5.849999999999989875 ) ) ;
#2091 = CARTESIAN_POINT ( 'NONE',  ( -9.858066664633883036, -1.612135949262833101, 9.548862081921404510 ) ) ;
#2092 = CARTESIAN_POINT ( 'NONE',  ( 9.837026868206066865, -5.012215536711392083, 19.34999999999996945 ) ) ;
#2093 = EDGE_CURVE ( 'NONE', #8307, #2751, #9346, .T. ) ;
#2094 = CARTESIAN_POINT ( 'NONE',  ( 5.284464991282756152, -15.10213328493384743, 45.42857142857143060 ) ) ;
#2095 = AXIS2_PLACEMENT_3D ( 'NONE', #4772, #6463, #6557 ) ;
#2096 = EDGE_CURVE ( 'NONE', #2369, #4723, #1540, .T. ) ;
#2097 =( NAMED_UNIT ( * ) SI_UNIT ( $, .STERADIAN. ) SOLID_ANGLE_UNIT ( ) );
#2098 = CARTESIAN_POINT ( 'NONE',  ( 15.06016580658428694, -5.404401153735007846, 24.57546914105500946 ) ) ;
#2099 = CARTESIAN_POINT ( 'NONE',  ( 9.899494936611718643, -9.899494936611608509, 21.00000000000000355 ) ) ;
#2100 = PRODUCT_DEFINITION_SHAPE ( 'NONE', 'NONE',  #10239 ) ;
#2101 = FACE_OUTER_BOUND ( 'NONE', #7126, .T. ) ;
#2102 = CARTESIAN_POINT ( 'NONE',  ( -5.420364854931999155, -15.49051278174644253, 40.07142857142857650 ) ) ;
#2103 = ORIENTED_EDGE ( 'NONE', *, *, #6989, .F. ) ;
#2104 = CARTESIAN_POINT ( 'NONE',  ( 9.837026868206066865, -5.012215536711392083, 13.34999999999998188 ) ) ;
#2105 = DIRECTION ( 'NONE',  ( -1.000000000000000000, 0.000000000000000000, 0.000000000000000000 ) ) ;
#2106 = FACE_OUTER_BOUND ( 'NONE', #8841, .T. ) ;
#2107 = PRESENTATION_LAYER_ASSIGNMENT (  '', '', ( #7384 ) ) ;
#2108 = CARTESIAN_POINT ( 'NONE',  ( 5.404401153735178376, -15.06016580658422477, 47.42453085894499765 ) ) ;
#2109 = CARTESIAN_POINT ( 'NONE',  ( 9.333916720356675967, 4.809394265263123636, 1.898862081921442790 ) ) ;
#2110 = CARTESIAN_POINT ( 'NONE',  ( 13.54758718765249803, 8.512513224245457977, 7.714285714285715301 ) ) ;
#2111 = APPLICATION_PROTOCOL_DEFINITION ( 'draft international standard', 'automotive_design', 1998, #3283 ) ;
#2112 = CARTESIAN_POINT ( 'NONE',  ( -9.899494936611716867, 9.899494936611610285, 24.00000000000000000 ) ) ;
#2113 = CARTESIAN_POINT ( 'NONE',  ( 4.619798703721856192, 13.59724543428036725, 39.06738800180213644 ) ) ;
#2114 = AXIS2_PLACEMENT_3D ( 'NONE', #3807, #8558, #6697 ) ;
#2115 = EDGE_LOOP ( 'NONE', ( #8839, #9422, #2671, #1888 ) ) ;
#2116 = FACE_OUTER_BOUND ( 'NONE', #145, .T. ) ;
#2117 = CARTESIAN_POINT ( 'NONE',  ( 5.297344310588354865, 15.53355953199867301, 27.06738800180213644 ) ) ;
#2118 = LINE ( 'NONE', #9875, #8996 ) ;
#2119 = EDGE_CURVE ( 'NONE', #4139, #3726, #6269, .T. ) ;
#2120 = CARTESIAN_POINT ( 'NONE',  ( 10.89658364409024749, 1.776620879821585897, 20.04886208192142050 ) ) ;
#2121 = CARTESIAN_POINT ( 'NONE',  ( -7.639999817571787588, 12.15899005565156266, 0.2142857142857168273 ) ) ;
#2122 = CARTESIAN_POINT ( 'NONE',  ( 9.355568503977840678, 4.766900247265305701, 9.900000000000019895 ) ) ;
#2123 = CARTESIAN_POINT ( 'NONE',  ( 9.377220287599001836, 4.724406229267492208, 11.90113791807857702 ) ) ;
#2124 = CARTESIAN_POINT ( 'NONE',  ( -158.0000000000000284, -13.00000000000001066, 1.592040838891559490E-15 ) ) ;
#2125 = CARTESIAN_POINT ( 'NONE',  ( 14.25515036105622535, -1.737328882695210241, 24.36118342676929416 ) ) ;
#2126 = EDGE_CURVE ( 'NONE', #9861, #928, #5621, .T. ) ;
#2127 = CARTESIAN_POINT ( 'NONE',  ( -1.642561882922479732, 10.37072757624895303, 15.29999999999997939 ) ) ;
#2128 = CARTESIAN_POINT ( 'NONE',  ( -13.96533075980324234, 8.621071003556515677, 49.78167371608785885 ) ) ;
#2129 = CARTESIAN_POINT ( 'NONE',  ( -1.727091770866549414, -10.90442828429184630, 7.950000000000040146 ) ) ;
#2130 = CARTESIAN_POINT ( 'NONE',  ( 8.512513224245308763, 13.54758718765259040, 25.28571428571428470 ) ) ;
#2131 = DIRECTION ( 'NONE',  ( -1.000000000000000000, -0.000000000000000000, -0.000000000000000000 ) ) ;
#2132 = CARTESIAN_POINT ( 'NONE',  ( 14.28433602490915000, -1.478298951650544479, 22.35310228751642114 ) ) ;
#2133 = CARTESIAN_POINT ( 'NONE',  ( -4.967534682030703586, 9.859792900771061852, -0.8488620819214613977 ) ) ;
#2134 = CARTESIAN_POINT ( 'NONE',  ( 9.873755945037075321, 1.513077731353044131, 6.051137918078538291 ) ) ;
#2135 = CARTESIAN_POINT ( 'NONE',  ( -165.6926619388180484, -2.040225341766198408, 12.83902055342544379 ) ) ;
#2136 = CARTESIAN_POINT ( 'NONE',  ( 15.06016580658428694, -5.404401153735007846, 42.57546914105501656 ) ) ;
#2137 = CARTESIAN_POINT ( 'NONE',  ( 4.623906867372411078, -13.21436662431711717, 39.42857142857143060 ) ) ;
#2138 = CARTESIAN_POINT ( 'NONE',  ( 13.92619789766827587, 1.441234910513398582, 6.146897712483580634 ) ) ;
#2139 = ORIENTED_EDGE ( 'NONE', *, *, #6893, .F. ) ;
#2140 = CARTESIAN_POINT ( 'NONE',  ( -8.404922754268618235, -13.61519076058357491, 6.281673716087846415 ) ) ;
#2141 = CARTESIAN_POINT ( 'NONE',  ( -10.84757329356279598, 11.77984370440671569, -1.110223024625157803E-13 ) ) ;
#2142 = CARTESIAN_POINT ( 'NONE',  ( 8.731428362939190890, -13.89598863503036164, 33.21428571428571530 ) ) ;
#2143 = CARTESIAN_POINT ( 'NONE',  ( -68.00000000000002842, 0.000000000000000000, 8.200000000000001066 ) ) ;
#2144 = CARTESIAN_POINT ( 'NONE',  ( -158.0000000000000284, -6.938893903907228378E-15, 0.000000000000000000 ) ) ;
#2145 = FACE_OUTER_BOUND ( 'NONE', #4650, .T. ) ;
#2146 = CARTESIAN_POINT ( 'NONE',  ( -9.865911304835474738, -1.562606840307925626, 8.549999999999963407 ) ) ;
#2147 = CARTESIAN_POINT ( 'NONE',  ( 6.717514421272239744, -6.717514421272154479, 1.500000000000001332 ) ) ;
#2148 = CARTESIAN_POINT ( 'NONE',  ( 1.642561882922480621, -10.37072757624891750, 10.80000000000003268 ) ) ;
#2149 = CARTESIAN_POINT ( 'NONE',  ( 1.707986654103998303, -16.32287076676380266, 19.64689771248358596 ) ) ;
#2150 = CARTESIAN_POINT ( 'NONE',  ( 5.420364854932001819, 15.49051278174644430, 37.07142857142857650 ) ) ;
#2151 = SURFACE_STYLE_USAGE ( .BOTH. , #8508 ) ;
#2152 = CARTESIAN_POINT ( 'NONE',  ( 11.69682198916835070, 11.51250119794901394, 17.50404056962643651 ) ) ;
#2153 = AXIS2_PLACEMENT_3D ( 'NONE', #3378, #1776, #9689 ) ;
#2154 = CIRCLE ( 'NONE', #8096, 1.535500000000000087 ) ;
#2155 = CARTESIAN_POINT ( 'NONE',  ( -4.623906867372410190, 13.21436662431711895, 24.42857142857143060 ) ) ;
#2156 = CARTESIAN_POINT ( 'NONE',  ( 8.512513224245308763, 13.54758718765259040, 7.285714285714284699 ) ) ;
#2157 = CARTESIAN_POINT ( 'NONE',  ( 16.30827793483735633, -1.837501619626142890, 44.35714285714287541 ) ) ;
#2158 = ORIENTED_EDGE ( 'NONE', *, *, #7634, .F. ) ;
#2159 = CARTESIAN_POINT ( 'NONE',  ( -7.806708723663830618, -7.806708723663901672, 17.25000000000003553 ) ) ;
#2160 = FACE_OUTER_BOUND ( 'NONE', #6889, .T. ) ;
#2161 = CARTESIAN_POINT ( 'NONE',  ( 15.49051278174637858, 5.420364854932174126, 43.92857142857143771 ) ) ;
#2162 = VECTOR ( 'NONE', #6837, 1000.000000000000000 ) ;
#2163 = CIRCLE ( 'NONE', #3319, 6.999999999999999112 ) ;
#2164 = CIRCLE ( 'NONE', #9761, 18.00000000000000355 ) ;
#2165 = CARTESIAN_POINT ( 'NONE',  ( 1.441234910513245149, 13.92619789766829008, 8.853102287516419366 ) ) ;
#2166 = CARTESIAN_POINT ( 'NONE',  ( -1.727091770866549414, -10.90442828429184630, 13.95000000000002593 ) ) ;
#2167 = CARTESIAN_POINT ( 'NONE',  ( 15.10213328493390783, -5.284464991282587398, 8.571428571428569398 ) ) ;
#2168 = CARTESIAN_POINT ( 'NONE',  ( 1.917699372585825790, 15.88516839912900203, 46.86118342676930126 ) ) ;
#2169 = APPLICATION_PROTOCOL_DEFINITION ( 'draft international standard', 'automotive_design', 1998, #6976 ) ;
#2170 = CARTESIAN_POINT ( 'NONE',  ( -10.15407889436378852, -10.15407889436390398, 28.50000000000000000 ) ) ;
#2171 = EDGE_CURVE ( 'NONE', #6156, #1436, #3387, .T. ) ;
#2172 = CIRCLE ( 'NONE', #2494, 15.44569104238500046 ) ;
#2173 = CARTESIAN_POINT ( 'NONE',  ( -13.17239914596754424, 4.743843029824683200, 21.57546914105500946 ) ) ;
#2174 = CIRCLE ( 'NONE', #3483, 0.9906000000000003691 ) ;
#2175 = COLOUR_RGB ( '', 0.72549020, 0.75294118, 0.79215686) ;
#2176 = CARTESIAN_POINT ( 'NONE',  ( -7.340858601237953529, -11.92174236212700222, 36.28167371608785174 ) ) ;
#2177 = ORIENTED_EDGE ( 'NONE', *, *, #4861, .T. ) ;
#2178 = PLANE ( 'NONE',  #459 ) ;
#2179 = CARTESIAN_POINT ( 'NONE',  ( 13.96533075980324234, -8.621071003556521006, 28.78167371608785174 ) ) ;
#2180 = CARTESIAN_POINT ( 'NONE',  ( -15.49051278174637858, -5.420364854932175014, 4.928571428571430602 ) ) ;
#2181 = CARTESIAN_POINT ( 'NONE',  ( 7.458344646081711105, -7.390897758835778930, 17.49886208192142689 ) ) ;
#2182 = CARTESIAN_POINT ( 'NONE',  ( -12.22833218042443271, 7.529642458189139909, 49.78167371608785885 ) ) ;
#2183 = CARTESIAN_POINT ( 'NONE',  ( -4.766900247265192014, -9.355568503977876205, 5.099999999999993427 ) ) ;
#2184 = CARTESIAN_POINT ( 'NONE',  ( 7.390897758835871301, -7.458344646081617846, 18.50113791807859087 ) ) ;
#2185 = DIRECTION ( 'NONE',  ( -0.000000000000000000, -0.000000000000000000, 1.000000000000000000 ) ) ;
#2186 = CARTESIAN_POINT ( 'NONE',  ( -8.841785722321695573, 13.82664651025757152, 50.21024514465927524 ) ) ;
#2187 = CARTESIAN_POINT ( 'NONE',  ( 5.012215536711512875, -9.837026868206002916, 1.650000000000006128 ) ) ;
#2188 = DIRECTION ( 'NONE',  ( -1.000000000000000000, 1.842239752758738928E-31, -1.780435181894459419E-32 ) ) ;
#2189 = CARTESIAN_POINT ( 'NONE',  ( 13.89774397934249706, 1.693770420379375308, 16.13881657323070584 ) ) ;
#2190 = CARTESIAN_POINT ( 'NONE',  ( 9.814260835641038128, -5.056896391392198709, 0.3511379180785880183 ) ) ;
#2191 = CARTESIAN_POINT ( 'NONE',  ( 9.375578539472099848, -1.533232399699986370, 9.201137918078538647 ) ) ;
#2192 = CARTESIAN_POINT ( 'NONE',  ( -167.1500000000000341, -0.1422832181819098096, 13.00000000000000178 ) ) ;
#2193 = CARTESIAN_POINT ( 'NONE',  ( -16.29368510291090288, 1.967016585148476215, 45.36118342676930837 ) ) ;
#2194 = CARTESIAN_POINT ( 'NONE',  ( 1.567502665446232957, 13.91197093850540156, 42.85714285714285410 ) ) ;
#2195 = CARTESIAN_POINT ( 'NONE',  ( -11.85413878919593422, -7.448449071214776396, 46.71428571428571530 ) ) ;
#2196 = ORIENTED_EDGE ( 'NONE', *, *, #2684, .F. ) ;
#2197 = CARTESIAN_POINT ( 'NONE',  ( -1.665163862719845067, -15.91362231745477374, 11.85310228751642470 ) ) ;
#2198 = DIRECTION ( 'NONE',  ( 0.9575619921529161527, -0.2882273949230689802, 3.311798021194119518E-34 ) ) ;
#2199 = CARTESIAN_POINT ( 'NONE',  ( -13.89598863503046111, 8.731428362939027465, 29.78571428571428825 ) ) ;
#2200 = DIRECTION ( 'NONE',  ( 1.000000000000000000, 0.000000000000000000, 0.000000000000000000 ) ) ;
#2201 = AXIS2_PLACEMENT_3D ( 'NONE', #4351, #1360, #5991 ) ;
#2202 = DIRECTION ( 'NONE',  ( 0.000000000000000000, -1.000000000000000000, 0.000000000000000000 ) ) ;
#2203 = CARTESIAN_POINT ( 'NONE',  ( -9.383039235653820143, 1.486127417882154411, 11.69999999999998863 ) ) ;
#2204 = CARTESIAN_POINT ( 'NONE',  ( 9.858066664633883036, 1.612135949262857526, 20.04886208192142050 ) ) ;
#2205 = CARTESIAN_POINT ( 'NONE',  ( -43.00000000000002842, 5.689893001204620728E-17, 8.200000000000009948 ) ) ;
#2206 = CARTESIAN_POINT ( 'NONE',  ( -13.89598863503046111, 8.731428362939027465, 41.78571428571430602 ) ) ;
#2207 = AXIS2_PLACEMENT_3D ( 'NONE', #8447, #1314, #9717 ) ;
#2208 = FILL_AREA_STYLE ('',( #6781 ) ) ;
#2209 = CARTESIAN_POINT ( 'NONE',  ( 15.91362231745475597, 1.665163862720026255, 24.14689771248357530 ) ) ;
#2210 = CARTESIAN_POINT ( 'NONE',  ( -15.10213328493390961, 5.284464991282586510, 17.57142857142856940 ) ) ;
#2211 = CARTESIAN_POINT ( 'NONE',  ( 8.282355133173227912, 13.51256563640100872, 48.73000000000003240 ) ) ;
#2212 = VERTEX_POINT ( 'NONE', #915 ) ;
#2213 = CARTESIAN_POINT ( 'NONE',  ( 1.642561882922480621, -10.37072757624891750, 10.80000000000003268 ) ) ;
#2214 = VERTEX_POINT ( 'NONE', #1891 ) ;
#2215 = CARTESIAN_POINT ( 'NONE',  ( -8.731428362939187338, 13.89598863503036164, 42.21428571428571530 ) ) ;
#2216 = CARTESIAN_POINT ( 'NONE',  ( 7.458344646081711105, -7.390897758835778930, 8.498862081921462419 ) ) ;
#2217 = CARTESIAN_POINT ( 'NONE',  ( 5.420364854932001819, 15.49051278174644430, 1.071428571428570287 ) ) ;
#2218 = CARTESIAN_POINT ( 'NONE',  ( 15.89939535829187278, 1.791431617653015174, 2.142857142857140573 ) ) ;
#2219 = CARTESIAN_POINT ( 'NONE',  ( 1.567502665446232957, 13.91197093850540156, 24.85714285714285765 ) ) ;
#2220 = CARTESIAN_POINT ( 'NONE',  ( 7.529642458189280241, -12.22833218042435099, 37.21832628391215536 ) ) ;
#2221 = CARTESIAN_POINT ( 'NONE',  ( 4.534861676072321046, -8.900167166472096270, 7.649999999999992362 ) ) ;
#2222 = CARTESIAN_POINT ( 'NONE',  ( -13.89774397934249706, -1.693770420379375974, 37.13881657323070584 ) ) ;
#2223 = EDGE_LOOP ( 'NONE', ( #7638, #5766 ) ) ;
#2224 = LINE ( 'NONE', #729, #9042 ) ;
#2225 = CARTESIAN_POINT ( 'NONE',  ( 11.51250119794888249, 11.69682198916847682, 27.49595943037356705 ) ) ;
#2226 = CARTESIAN_POINT ( 'NONE',  ( -11.31370849898482156, 11.31370849898469544, 5.999999999999998224 ) ) ;
#2227 = CARTESIAN_POINT ( 'NONE',  ( -4.579542530753125895, 8.877401133907090625, 10.14886208192142725 ) ) ;
#2228 = EDGE_CURVE ( 'NONE', #6421, #9282, #4166, .T. ) ;
#2229 = CARTESIAN_POINT ( 'NONE',  ( 15.14410076328353227, -5.164528828830166063, 28.56738800180213644 ) ) ;
#2230 = CARTESIAN_POINT ( 'NONE',  ( -10.36326688006724162, 1.689666864740236862, 10.70113791807854220 ) ) ;
#2231 = DIRECTION ( 'NONE',  ( 3.081487911019577365E-32, 0.4999999999999990008, -0.8660254037844391517 ) ) ;
#2232 = CARTESIAN_POINT ( 'NONE',  ( -13.92619789766827054, -1.441234910513399470, 45.14689771248358596 ) ) ;
#2233 = APPLICATION_CONTEXT ( 'automotive_design' ) ;
#2234 = CARTESIAN_POINT ( 'NONE',  ( 10.90442828429184274, 1.727091770866679310, 1.049999999999966738 ) ) ;
#2235 = CARTESIAN_POINT ( 'NONE',  ( 2.000000000000001776, -1.773042676681352292, -1.110223024625156540E-13 ) ) ;
#2236 = CARTESIAN_POINT ( 'NONE',  ( -11.78653521626494793, -7.556039541191465148, 30.71024514465928235 ) ) ;
#2237 = CARTESIAN_POINT ( 'NONE',  ( 4.355403765523470305, 8.442910196168369907, 14.60113791807856920 ) ) ;
#2238 = CARTESIAN_POINT ( 'NONE',  ( -9.375578539472099848, 1.533232399700011461, 4.701137918078535982 ) ) ;
#2239 = FACE_OUTER_BOUND ( 'NONE', #413, .T. ) ;
#2240 = CARTESIAN_POINT ( 'NONE',  ( -15.53355953199861794, -5.297344310588530725, 44.93261199819787777 ) ) ;
#2241 = CARTESIAN_POINT ( 'NONE',  ( 10.15407889436379030, 10.15407889436390576, 37.50000000000002842 ) ) ;
#2242 = CARTESIAN_POINT ( 'NONE',  ( 12.08964793087886314, -7.750357176954162597, 0.7897548553407187644 ) ) ;
#2243 = ORIENTED_EDGE ( 'NONE', *, *, #5831, .T. ) ;
#2244 = CYLINDRICAL_SURFACE ( 'NONE', #10022, 1.816100000000000270 ) ;
#2245 = CARTESIAN_POINT ( 'NONE',  ( -11.60466159355861926, -11.60466159355875249, 34.50000000000000000 ) ) ;
#2246 = DIRECTION ( 'NONE',  ( 1.000000000000000000, 4.755747939841215952E-17, -0.000000000000000000 ) ) ;
#2247 = LINE ( 'NONE', #22, #4477 ) ;
#2248 = DIRECTION ( 'NONE',  ( -0.000000000000000000, 0.000000000000000000, 1.000000000000000000 ) ) ;
#2249 = CARTESIAN_POINT ( 'NONE',  ( -7.063212654743466601, -7.063212654743534991, 8.250000000000028422 ) ) ;
#2250 = CARTESIAN_POINT ( 'NONE',  ( 8.442910196168311288, 4.355403765523576887, 16.89886208192141126 ) ) ;
#2251 = EDGE_CURVE ( 'NONE', #879, #8995, #3817, .T. ) ;
#2252 = DIRECTION ( 'NONE',  ( 0.000000000000000000, 0.000000000000000000, 1.000000000000000000 ) ) ;
#2253 = CARTESIAN_POINT ( 'NONE',  ( 13.54758718765249803, 8.512513224245457977, 37.71428571428571530 ) ) ;
#2254 = CARTESIAN_POINT ( 'NONE',  ( 5.164528828830335705, -15.14410076328347543, 25.43261199819786711 ) ) ;
#2255 = CARTESIAN_POINT ( 'NONE',  ( 13.89598863503046111, -8.731428362939032795, 14.78571428571429358 ) ) ;
#2256 = CARTESIAN_POINT ( 'NONE',  ( -0.3453160816774686892, 15.99627321608801367, 48.73000000000002530 ) ) ;
#2257 = CARTESIAN_POINT ( 'NONE',  ( 10.37072757624895836, -1.642561882922356498, 13.19999999999998863 ) ) ;
#2258 = VERTEX_POINT ( 'NONE', #3281 ) ;
#2259 = CARTESIAN_POINT ( 'NONE',  ( 15.10213328493390783, -5.284464991282587398, 38.57142857142857650 ) ) ;
#2260 = EDGE_CURVE ( 'NONE', #7109, #7986, #7260, .T. ) ;
#2261 = CARTESIAN_POINT ( 'NONE',  ( -1.689666864740335228, 10.36326688006722740, 13.29886208192143471 ) ) ;
#2262 = CARTESIAN_POINT ( 'NONE',  ( -1.837501619626328297, 16.30827793483733856, 6.642857142857143238 ) ) ;
#2263 = CARTESIAN_POINT ( 'NONE',  ( -13.61519076058348254, -8.404922754268771001, 44.71832628391215536 ) ) ;
#2264 = ADVANCED_FACE ( 'NONE', ( #8085 ), #5129, .F. ) ;
#2265 = CARTESIAN_POINT ( 'NONE',  ( -4.623906867372410190, 13.21436662431711895, 18.42857142857143415 ) ) ;
#2266 = CARTESIAN_POINT ( 'NONE',  ( -1.693770420379220099, -13.89774397934251837, 31.86118342676929416 ) ) ;
#2267 = CARTESIAN_POINT ( 'NONE',  ( -7.063212654743467489, -7.063212654743533214, 11.24999999999999467 ) ) ;
#2268 = AXIS2_PLACEMENT_3D ( 'NONE', #2992, #6135, #9311 ) ;
#2269 = ORIENTED_EDGE ( 'NONE', *, *, #5485, .T. ) ;
#2270 = CARTESIAN_POINT ( 'NONE',  ( 14.28433602490915000, -1.478298951650544479, 40.35310228751642825 ) ) ;
#2271 = ORIENTED_EDGE ( 'NONE', *, *, #6815, .F. ) ;
#2272 = CYLINDRICAL_SURFACE ( 'NONE', #5880, 3.500000000000000000 ) ;
#2273 = CARTESIAN_POINT ( 'NONE',  ( -5.297344310588352201, -15.53355953199867301, 18.06738800180213644 ) ) ;
#2274 = CARTESIAN_POINT ( 'NONE',  ( 15.89939535829187278, 1.791431617653015174, 8.142857142857145902 ) ) ;
#2275 = CARTESIAN_POINT ( 'NONE',  ( 9.390499931835536884, -1.439022436064273158, 8.198862081921454603 ) ) ;
#2276 = CARTESIAN_POINT ( 'NONE',  ( 5.404401153735178376, -15.06016580658422477, 29.42453085894499765 ) ) ;
#2277 = CARTESIAN_POINT ( 'NONE',  ( -9.355568503977838901, -4.766900247265280832, 2.400000000000013234 ) ) ;
#2278 = CARTESIAN_POINT ( 'NONE',  ( -7.842167650704559456, -7.771249796623180828, 13.25113791807857311 ) ) ;
#2279 = DIRECTION ( 'NONE',  ( 0.000000000000000000, -8.191099868251446680E-34, -1.000000000000000000 ) ) ;
#2280 = CARTESIAN_POINT ( 'NONE',  ( -11.92174236212692051, -7.340858601238089420, 44.71832628391215536 ) ) ;
#2281 = SHAPE_REPRESENTATION_RELATIONSHIP ( 'NONE' , 'NONE' ,  #6629, #4260 ) ;
#2282 = PRESENTATION_LAYER_ASSIGNMENT (  '', '', ( #4756 ) ) ;
#2283 = CARTESIAN_POINT ( 'NONE',  ( 13.96533075980324234, -8.621071003556521006, 46.78167371608785885 ) ) ;
#2284 = CARTESIAN_POINT ( 'NONE',  ( 10.37072757624895836, -1.642561882922355609, 4.199999999999981526 ) ) ;
#2285 = CARTESIAN_POINT ( 'NONE',  ( 11.60466159355862104, 11.60466159355875071, 31.50000000000001421 ) ) ;
#2286 = EDGE_CURVE ( 'NONE', #9360, #3923, #3473, .T. ) ;
#2287 = PLANE ( 'NONE',  #3033 ) ;
#2288 = AXIS2_PLACEMENT_3D ( 'NONE', #6127, #8565, #8671 ) ;
#2289 = CARTESIAN_POINT ( 'NONE',  ( -4.619798703721853528, -13.59724543428036725, 24.06738800180213644 ) ) ;
#2290 = CARTESIAN_POINT ( 'NONE',  ( 9.814260835641038128, -5.056896391392198709, 9.351137918078563871 ) ) ;
#2291 = CARTESIAN_POINT ( 'NONE',  ( -7.098671581784199880, -7.027753727702804376, 7.251137918078588207 ) ) ;
#2292 = CARTESIAN_POINT ( 'NONE',  ( -167.0388786721946701, -0.6964701277567462157, 12.98197609665553287 ) ) ;
#2293 = CARTESIAN_POINT ( 'NONE',  ( -13.82664651025767100, 8.841785722321537477, 45.78975485534073897 ) ) ;
#2294 = CARTESIAN_POINT ( 'NONE',  ( -1.693770420379220099, -13.89774397934251837, 1.861183426769295490 ) ) ;
#2295 = CARTESIAN_POINT ( 'NONE',  ( 13.59724543428031573, 4.619798703722006294, -0.06738800180213055935 ) ) ;
#2296 = ORIENTED_EDGE ( 'NONE', *, *, #2974, .T. ) ;
#2297 = CARTESIAN_POINT ( 'NONE',  ( 1.967016585148662289, -16.29368510291087091, 11.63881657323070939 ) ) ;
#2298 = CARTESIAN_POINT ( 'NONE',  ( 0.000000000000000000, 5.592146987065130084E-32, 0.000000000000000000 ) ) ;
#2299 = CARTESIAN_POINT ( 'NONE',  ( -1.791431617652833763, -15.89939535829188877, 45.85714285714286120 ) ) ;
#2300 = CARTESIAN_POINT ( 'NONE',  ( 0.000000000000000000, 0.8865213383406900238, 1.535499999999967446 ) ) ;
#2301 = DIRECTION ( 'NONE',  ( -1.840628461782073167E-32, -6.938893903907220674E-18, -1.000000000000000000 ) ) ;
#2302 = CARTESIAN_POINT ( 'NONE',  ( 4.490180821391514421, -8.922933199037132113, 0.6511379180785785703 ) ) ;
#2303 = CARTESIAN_POINT ( 'NONE',  ( 7.027753727702739539, 7.098671581784288698, 19.74886208192143044 ) ) ;
#2304 = DIRECTION ( 'NONE',  ( 0.7063021515967560227, 0.7063021515967630171, 0.04769215134145720486 ) ) ;
#2305 = CARTESIAN_POINT ( 'NONE',  ( 15.91362231745475597, 1.665163862720026255, 18.14689771248357530 ) ) ;
#2306 = DIRECTION ( 'NONE',  ( 0.000000000000000000, 0.000000000000000000, 1.000000000000000000 ) ) ;
#2307 = CARTESIAN_POINT ( 'NONE',  ( -8.620103694221995738, -13.47998361472161299, 20.28975485534072121 ) ) ;
#2308 = ORIENTED_EDGE ( 'NONE', *, *, #5817, .T. ) ;
#2309 = CARTESIAN_POINT ( 'NONE',  ( 1.837501619626330074, -16.30827793483733501, 15.64285714285714235 ) ) ;
#2310 = DIRECTION ( 'NONE',  ( 0.000000000000000000, -1.000000000000000000, 0.000000000000000000 ) ) ;
#2311 = CARTESIAN_POINT ( 'NONE',  ( 13.89598863503046111, -8.731428362939032795, 2.785714285714284255 ) ) ;
#2312 = DIRECTION ( 'NONE',  ( 0.000000000000000000, 1.000000000000000000, 0.000000000000000000 ) ) ;
#2313 = CARTESIAN_POINT ( 'NONE',  ( -9.859792900771106261, 4.967534682030606774, 6.848862081921402556 ) ) ;
#2314 = CARTESIAN_POINT ( 'NONE',  ( -5.543385399275643444, -15.44746603149420494, 44.07546914105503078 ) ) ;
#2315 = CONTEXT_DEPENDENT_SHAPE_REPRESENTATION ( #5008, #6784 ) ;
#2316 = CARTESIAN_POINT ( 'NONE',  ( 7.639999817571788476, -12.15899005565156266, 45.21428571428572951 ) ) ;
#2317 = CARTESIAN_POINT ( 'NONE',  ( -6.717514421272238856, 6.717514421272181124, 6.000000000000005329 ) ) ;
#2318 = CARTESIAN_POINT ( 'NONE',  ( 7.806708723663831506, 7.806708723663930982, 12.75000000000000533 ) ) ;
#2319 = ORIENTED_EDGE ( 'NONE', *, *, #8480, .F. ) ;
#2320 = CARTESIAN_POINT ( 'NONE',  ( -12.22833218042443271, 7.529642458189139909, 43.78167371608784464 ) ) ;
#2321 = VECTOR ( 'NONE', #8550, 1000.000000000000000 ) ;
#2322 = EDGE_LOOP ( 'NONE', ( #3299, #2334, #4781, #8008 ) ) ;
#2323 = CIRCLE ( 'NONE', #9921, 18.00000000000001776 ) ;
#2324 = DIRECTION ( 'NONE',  ( -1.000000000000000000, -0.000000000000000000, -0.000000000000000000 ) ) ;
#2325 = CARTESIAN_POINT ( 'NONE',  ( 5.297344310588354865, 15.53355953199867301, 21.06738800180213644 ) ) ;
#2326 = AXIS2_PLACEMENT_3D ( 'NONE', #4570, #9220, #7774 ) ;
#2327 = CARTESIAN_POINT ( 'NONE',  ( 5.420364854932000931, 15.49051278174644075, 1.071428571428570065 ) ) ;
#2328 = CARTESIAN_POINT ( 'NONE',  ( -1.665163862719845067, -15.91362231745477374, 29.85310228751642470 ) ) ;
#2329 = FACE_OUTER_BOUND ( 'NONE', #3355, .T. ) ;
#2330 = CARTESIAN_POINT ( 'NONE',  ( -7.424621202458789426, 7.424621202458723701, 9.000000000000007105 ) ) ;
#2331 = FACE_OUTER_BOUND ( 'NONE', #6749, .T. ) ;
#2332 = STYLED_ITEM ( 'NONE', ( #9456 ), #7008 ) ;
#2333 =( LENGTH_UNIT ( ) NAMED_UNIT ( * ) SI_UNIT ( .MILLI., .METRE. ) );
#2334 = ORIENTED_EDGE ( 'NONE', *, *, #7588, .F. ) ;
#2335 = CARTESIAN_POINT ( 'NONE',  ( 10.06191849875406064, 10.24623928997363187, 3.495959430373559940 ) ) ;
#2336 = CARTESIAN_POINT ( 'NONE',  ( 0.2000000000000057288, 0.000000000000000000, 0.000000000000000000 ) ) ;
#2337 = CARTESIAN_POINT ( 'NONE',  ( 14.28433602490915000, -1.478298951650544479, 28.35310228751642825 ) ) ;
#2338 = CARTESIAN_POINT ( 'NONE',  ( 9.814260835641038128, -5.056896391392198709, 3.351137918078579858 ) ) ;
#2339 = CARTESIAN_POINT ( 'NONE',  ( 7.098671581784200768, 7.027753727702831021, 17.75113791807856245 ) ) ;
#2340 = CARTESIAN_POINT ( 'NONE',  ( -164.4413679183172121, -2.080883175690475539, 12.83240817167530246 ) ) ;
#2341 = CARTESIAN_POINT ( 'NONE',  ( -13.17239914596754424, 4.743843029824683200, 9.575469141055007682 ) ) ;
#2342 = CLOSED_SHELL ( 'NONE', ( #1235, #3952, #3173, #1659, #7271, #4523 ) ) ;
#2343 = CARTESIAN_POINT ( 'NONE',  ( 13.59724543428031573, 4.619798703722006294, 11.93261199819786178 ) ) ;
#2344 = ORIENTED_EDGE ( 'NONE', *, *, #3789, .T. ) ;
#2345 = VECTOR ( 'NONE', #2035, 1000.000000000000000 ) ;
#2346 = CARTESIAN_POINT ( 'NONE',  ( -8.841785722321695573, 13.82664651025757152, 8.210245144659282346 ) ) ;
#2347 = CARTESIAN_POINT ( 'NONE',  ( 14.00000000000000533, 1.971681346627238735E-16, -1.610000000000000098 ) ) ;
#2348 = CARTESIAN_POINT ( 'NONE',  ( -13.54758718765249625, -8.512513224245459753, 46.71428571428571530 ) ) ;
#2349 = CYLINDRICAL_SURFACE ( 'NONE', #5335, 17.72919999999999874 ) ;
#2350 = CARTESIAN_POINT ( 'NONE',  ( -43.00000000000002842, 6.933347799794049071E-30, -9.629649721936179265E-31 ) ) ;
#2351 = CARTESIAN_POINT ( 'NONE',  ( 6.717514421272239744, -6.717514421272154479, 16.50000000000001421 ) ) ;
#2352 = CARTESIAN_POINT ( 'NONE',  ( -9.390499931835536884, 1.439022436064298249, 15.69886208192145816 ) ) ;
#2353 = CARTESIAN_POINT ( 'NONE',  ( 11.48991645990273724, -11.34085470199652512, -1.270000000000007123 ) ) ;
#2354 = CARTESIAN_POINT ( 'NONE',  ( -8.620103694221995738, -13.47998361472161299, 32.28975485534072476 ) ) ;
#2355 = LINE ( 'NONE', #3229, #7258 ) ;
#2356 = CARTESIAN_POINT ( 'NONE',  ( -11.69682198916834892, -11.51250119794901394, 38.50404056962644006 ) ) ;
#2357 = CARTESIAN_POINT ( 'NONE',  ( 1.791431617652837316, 15.89939535829188877, 18.85714285714285765 ) ) ;
#2358 = DIRECTION ( 'NONE',  ( 0.000000000000000000, -1.000000000000000000, 9.714451465470119729E-16 ) ) ;
#2359 = CIRCLE ( 'NONE', #2542, 13.00000000000000355 ) ;
#2360 = CARTESIAN_POINT ( 'NONE',  ( 8.512513224245308763, 13.54758718765259040, 7.285714285714284699 ) ) ;
#2361 = CARTESIAN_POINT ( 'NONE',  ( -1.689666864740335228, 10.36326688006723451, 7.298862081921430267 ) ) ;
#2362 = CARTESIAN_POINT ( 'NONE',  ( 11.92174236212692229, 7.340858601238088532, 41.71832628391215536 ) ) ;
#2363 = CARTESIAN_POINT ( 'NONE',  ( 11.60466159355862104, 11.60466159355875071, 13.50000000000000178 ) ) ;
#2364 = SHAPE_DEFINITION_REPRESENTATION ( #5902, #5586 ) ;
#2365 = CARTESIAN_POINT ( 'NONE',  ( -1.567502665446231180, -13.91197093850540334, 33.85714285714285410 ) ) ;
#2366 = CARTESIAN_POINT ( 'NONE',  ( -13.92619789766827054, -1.441234910513399470, 39.14689771248358596 ) ) ;
#2367 = CARTESIAN_POINT ( 'NONE',  ( 1.486127417882244783, -9.383039235653791721, 13.80000000000003446 ) ) ;
#2368 = CARTESIAN_POINT ( 'NONE',  ( 10.90442828429183919, 1.727091770866679532, 19.04999999999997939 ) ) ;
#2369 = VERTEX_POINT ( 'NONE', #7988 ) ;
#2370 = CARTESIAN_POINT ( 'NONE',  ( 4.623906867372411078, -13.21436662431711717, 9.428571428571425272 ) ) ;
#2371 = EDGE_LOOP ( 'NONE', ( #962, #2319, #834 ) ) ;
#2372 = CARTESIAN_POINT ( 'NONE',  ( 0.000000000000000000, -1.018491042385001544, 0.000000000000000000 ) ) ;
#2373 = CARTESIAN_POINT ( 'NONE',  ( -8.404922754268618235, -13.61519076058357491, 30.28167371608785530 ) ) ;
#2374 = CARTESIAN_POINT ( 'NONE',  ( 11.60466159355861926, 11.60466159355874716, 19.50000000000000355 ) ) ;
#2375 = CARTESIAN_POINT ( 'NONE',  ( -13.96533075980324234, 8.621071003556515677, 25.78167371608785530 ) ) ;
#2376 = CARTESIAN_POINT ( 'NONE',  ( 9.355568503977840678, 4.766900247265305701, 0.9000000000000119016 ) ) ;
#2377 = CARTESIAN_POINT ( 'NONE',  ( 7.806708723663831506, 7.806708723663925653, 9.749999999999982236 ) ) ;
#2378 = EDGE_CURVE ( 'NONE', #728, #3550, #1331, .T. ) ;
#2379 = DIRECTION ( 'NONE',  ( -0.7071067811865350272, 5.791982262216934087E-34, 0.7071067811865598962 ) ) ;
#2380 = AXIS2_PLACEMENT_3D ( 'NONE', #788, #4715, #1569 ) ;
#2381 = B_SPLINE_CURVE_WITH_KNOTS ( 'NONE', 3,
 ( #7253, #8759, #9543, #7306, #8820, #123, #4778, #3333, #2450, #175, #4058, #1687, #3228, #228, #6470, #9648, #5550, #3381, #8709, #5596, #5744, #4829, #7982, #75, #8079, #9693, #4205, #4157, #8913, #1064 ),
 .UNSPECIFIED., .F., .F.,
 ( 4, 2, 2, 2, 2, 2, 2, 2, 2, 2, 2, 2, 2, 2, 4 ),
 ( 5.712404575677604335E-19, 0.0004208408401708223071, 0.0008416816803416437469, 0.001262522520512465458, 0.001683363360683286626, 0.002525045041024870634, 0.003366726721366455292, 0.003787567561537246753, 0.004208408401708039516, 0.004629249241878830544, 0.005050090082049622439, 0.005470930922220414334, 0.005891771762391206230, 0.006312612602561998125, 0.006733453442732789153 ),
 .UNSPECIFIED. ) ;
#2382 = ORIENTED_EDGE ( 'NONE', *, *, #9479, .T. ) ;
#2383 = CARTESIAN_POINT ( 'NONE',  ( 1.737328882695370558, -14.25515036105620581, 17.63881657323070939 ) ) ;
#2384 = CARTESIAN_POINT ( 'NONE',  ( 1.642561882922480621, -10.37072757624892638, 16.80000000000003624 ) ) ;
#2385 = CARTESIAN_POINT ( 'NONE',  ( 16.30827793483735633, -1.837501619626142890, 14.35714285714285587 ) ) ;
#2386 = CARTESIAN_POINT ( 'NONE',  ( 6.976602070941136269, -13.58603705635637304, -1.270000000000007123 ) ) ;
#2387 = CARTESIAN_POINT ( 'NONE',  ( 10.91227292449344155, 1.677562661911773390, 3.051137918078546285 ) ) ;
#2388 = CARTESIAN_POINT ( 'NONE',  ( -1.612135949262737844, -9.858066664633888365, 9.951137918078590161 ) ) ;
#2389 = EDGE_CURVE ( 'NONE', #1237, #4901, #9655, .T. ) ;
#2390 = CARTESIAN_POINT ( 'NONE',  ( -83.00000000000001421, 9.797174393178825657E-16, -8.000000000000000000 ) ) ;
#2391 = CARTESIAN_POINT ( 'NONE',  ( 1.693770420379222319, 13.89774397934251837, 4.861183426769296823 ) ) ;
#2392 = CARTESIAN_POINT ( 'NONE',  ( -9.809645194534070356, 9.989344678689256796, 10.00404056962643651 ) ) ;
#2393 = EDGE_LOOP ( 'NONE', ( #702, #4065, #7859, #9267 ) ) ;
#2394 = CARTESIAN_POINT ( 'NONE',  ( 15.88516839912898071, 1.917699372586004092, 16.13881657323070584 ) ) ;
#2395 = FACE_OUTER_BOUND ( 'NONE', #1423, .T. ) ;
#2396 = CARTESIAN_POINT ( 'NONE',  ( -1.837501619626328297, 16.30827793483733856, 48.64285714285716011 ) ) ;
#2397 = CARTESIAN_POINT ( 'NONE',  ( 14.00000000000000533, 1.318767078788482996E-33, 1.610000000000000098 ) ) ;
#2398 = LINE ( 'NONE', #9388, #5266 ) ;
#2399 = CARTESIAN_POINT ( 'NONE',  ( 8.464561979789474222, 4.312909747525755400, 18.90000000000002700 ) ) ;
#2400 = CARTESIAN_POINT ( 'NONE',  ( -6.717514421272238856, 6.717514421272180236, 9.000000000000007105 ) ) ;
#2401 = CARTESIAN_POINT ( 'NONE',  ( -13.54758718765249625, -8.512513224245459753, 34.71428571428571530 ) ) ;
#2402 = CYLINDRICAL_SURFACE ( 'NONE', #8419, 18.00000000000000355 ) ;
#2403 = CARTESIAN_POINT ( 'NONE',  ( -1.917699372585823570, -15.88516839912900558, 25.86118342676929416 ) ) ;
#2404 = DIRECTION ( 'NONE',  ( -1.000000000000000000, 0.000000000000000000, 0.000000000000000000 ) ) ;
#2405 = CARTESIAN_POINT ( 'NONE',  ( 5.543385399275644332, 15.44746603149420494, 35.07546914105501656 ) ) ;
#2406 = ORIENTED_EDGE ( 'NONE', *, *, #4728, .F. ) ;
#2407 = CARTESIAN_POINT ( 'NONE',  ( 1.837501619626330074, -16.30827793483733501, 21.64285714285714590 ) ) ;
#2408 = CARTESIAN_POINT ( 'NONE',  ( 4.931155215468822739, 15.20764708138552912, 48.73000000000003240 ) ) ;
#2409 = CARTESIAN_POINT ( 'NONE',  ( -8.512513224245306986, -13.54758718765259218, 4.285714285714288252 ) ) ;
#2410 = EDGE_CURVE ( 'NONE', #6566, #6181, #4234, .T. ) ;
#2411 = CARTESIAN_POINT ( 'NONE',  ( 8.922933199037192509, -4.490180821391407839, 2.348862081921457623 ) ) ;
#2412 = EDGE_CURVE ( 'NONE', #1541, #999, #1993, .T. ) ;
#2413 = ADVANCED_BREP_SHAPE_REPRESENTATION ( '', ( #254, #3995 ), #6945 ) ;
#2414 = CARTESIAN_POINT ( 'NONE',  ( 9.859792900771104485, -4.967534682030585458, 5.348862081921449629 ) ) ;
#2415 = CARTESIAN_POINT ( 'NONE',  ( -12.08964793087886314, 7.750357176954159932, 45.78975485534073897 ) ) ;
#2416 = CARTESIAN_POINT ( 'NONE',  ( 13.89598863503046111, -8.731428362939032795, 20.78571428571429180 ) ) ;
#2417 = CARTESIAN_POINT ( 'NONE',  ( 1.567502665446232957, 13.91197093850540156, 36.85714285714286120 ) ) ;
#2418 = CARTESIAN_POINT ( 'NONE',  ( 7.556039541191335474, 11.78653521626503320, 35.28975485534072476 ) ) ;
#2419 = CARTESIAN_POINT ( 'NONE',  ( 1.562606840307832146, 9.865911304835501383, 6.449999999999970868 ) ) ;
#2420 = CARTESIAN_POINT ( 'NONE',  ( 7.806708723663831506, 7.806708723663925653, 15.74999999999996803 ) ) ;
#2421 = ORIENTED_EDGE ( 'NONE', *, *, #1932, .T. ) ;
#2422 = CARTESIAN_POINT ( 'NONE',  ( -7.750357176954294935, 12.08964793087877787, 50.21024514465927524 ) ) ;
#2423 = ORIENTED_EDGE ( 'NONE', *, *, #1818, .T. ) ;
#2424 = CARTESIAN_POINT ( 'NONE',  ( -83.00000000000001421, 0.000000000000000000, 13.00000000000000000 ) ) ;
#2425 = CARTESIAN_POINT ( 'NONE',  ( 15.49051278174637858, 5.420364854932174126, 13.92857142857143060 ) ) ;
#2426 = CARTESIAN_POINT ( 'NONE',  ( -16.32287076676382398, 1.707986654103809343, 25.35310228751642470 ) ) ;
#2427 = DIRECTION ( 'NONE',  ( -1.000000000000000000, 0.000000000000000000, 0.000000000000000000 ) ) ;
#2428 = CARTESIAN_POINT ( 'NONE',  ( 5.012215536711511987, -9.837026868205999364, 1.650000000000006128 ) ) ;
#2429 = DIRECTION ( 'NONE',  ( 1.000000000000000000, 0.000000000000000000, 0.000000000000000000 ) ) ;
#2430 =( NAMED_UNIT ( * ) PLANE_ANGLE_UNIT ( ) SI_UNIT ( $, .RADIAN. ) );
#2431 = ORIENTED_EDGE ( 'NONE', *, *, #9868, .F. ) ;
#2432 = CARTESIAN_POINT ( 'NONE',  ( 1.737328882695370558, -14.25515036105620581, 11.63881657323070939 ) ) ;
#2433 = EDGE_CURVE ( 'NONE', #6370, #5215, #9264, .T. ) ;
#2434 = CARTESIAN_POINT ( 'NONE',  ( -7.806708723663831506, -7.806708723663902560, 11.24999999999999467 ) ) ;
#2435 = CARTESIAN_POINT ( 'NONE',  ( -165.8275777035124747, 1.431488817417934101, 12.92108529057806798 ) ) ;
#2436 = CARTESIAN_POINT ( 'NONE',  ( -7.842167650704559456, -7.771249796623176387, 1.251137918078559563 ) ) ;
#2437 = CARTESIAN_POINT ( 'NONE',  ( 9.873755945037075321, 1.513077731353043243, 15.05113791807855961 ) ) ;
#2438 = EDGE_CURVE ( 'NONE', #6370, #7745, #3691, .T. ) ;
#2439 =( GEOMETRIC_REPRESENTATION_CONTEXT ( 3 ) GLOBAL_UNCERTAINTY_ASSIGNED_CONTEXT ( ( #8673 ) ) GLOBAL_UNIT_ASSIGNED_CONTEXT ( ( #1544, #1592, #3966 ) ) REPRESENTATION_CONTEXT ( 'NONE', 'WORKASPACE' ) );
#2440 = DIRECTION ( 'NONE',  ( 0.000000000000000000, 6.938893903907220674E-18, 1.000000000000000000 ) ) ;
#2441 = CARTESIAN_POINT ( 'NONE',  ( 4.865839792409144771, 13.51115193377589740, 5.075469141055008571 ) ) ;
#2442 = CARTESIAN_POINT ( 'NONE',  ( 12.08964793087886314, -7.750357176954162597, 12.78975485534072121 ) ) ;
#2443 = ORIENTED_EDGE ( 'NONE', *, *, #5713, .T. ) ;
#2444 = DIRECTION ( 'NONE',  ( 1.540743955509789230E-32, 0.8660254037844380415, -0.5000000000000012212 ) ) ;
#2445 = CARTESIAN_POINT ( 'NONE',  ( -13.54758718765249625, -8.512513224245459753, 40.71428571428571530 ) ) ;
#2446 = PRODUCT_DEFINITION_FORMATION_WITH_SPECIFIED_SOURCE ( 'ANY', '', #3433, .NOT_KNOWN. ) ;
#2447 = CARTESIAN_POINT ( 'NONE',  ( -165.5332536431789094, -1.565195349311612416, 12.90549919778201904 ) ) ;
#2448 = CARTESIAN_POINT ( 'NONE',  ( -1.562606840307830591, -9.865911304835478290, 13.95000000000002593 ) ) ;
#2449 = CARTESIAN_POINT ( 'NONE',  ( -4.534861676072319270, 8.900167166472121139, 3.149999999999957723 ) ) ;
#2450 = CARTESIAN_POINT ( 'NONE',  ( -166.6189502573242578, 1.421653495296104408, 12.92241587668698166 ) ) ;
#2451 = CARTESIAN_POINT ( 'NONE',  ( 8.620103694221997515, 13.47998361472160767, 23.28975485534072121 ) ) ;
#2452 = CARTESIAN_POINT ( 'NONE',  ( 8.900167166472158442, -4.534861676072210024, 4.350000000000036948 ) ) ;
#2453 = ADVANCED_FACE ( 'NONE', ( #390 ), #2856, .F. ) ;
#2454 = CARTESIAN_POINT ( 'NONE',  ( -11.22385875690717327, 11.40355824106234550, 40.00404056962644006 ) ) ;
#2455 = ORIENTED_EDGE ( 'NONE', *, *, #967, .T. ) ;
#2456 = CARTESIAN_POINT ( 'NONE',  ( -1.837501619626328297, 16.30827793483733856, 36.64285714285714590 ) ) ;
#2457 = CARTESIAN_POINT ( 'NONE',  ( 3.853817051969782970, 14.41361677514167283, 2.166671187435320663E-31 ) ) ;
#2458 = CARTESIAN_POINT ( 'NONE',  ( -13.89598863503046111, 8.731428362939027465, 5.785714285714282035 ) ) ;
#2459 = CARTESIAN_POINT ( 'NONE',  ( 4.579542530753127672, -8.877401133907065756, 5.648862081921440570 ) ) ;
#2460 = CARTESIAN_POINT ( 'NONE',  ( 1.689666864740335894, -10.36326688006720786, 17.79886208192143471 ) ) ;
#2461 = CARTESIAN_POINT ( 'NONE',  ( 7.458344646081711105, -7.390897758835778930, 14.49886208192142867 ) ) ;
#2462 = CARTESIAN_POINT ( 'NONE',  ( -8.621071003556675549, 13.96533075980314642, -1.781673716087850634 ) ) ;
#2463 = CARTESIAN_POINT ( 'NONE',  ( -11.60466159355861926, -11.60466159355875249, 10.50000000000000533 ) ) ;
#2464 = CARTESIAN_POINT ( 'NONE',  ( 7.639999817571788476, -12.15899005565156266, 33.21428571428571530 ) ) ;
#2465 = CARTESIAN_POINT ( 'NONE',  ( 12.08964793087886314, -7.750357176954162597, 42.78975485534072476 ) ) ;
#2466 = LINE ( 'NONE', #6532, #6097 ) ;
#2467 = CARTESIAN_POINT ( 'NONE',  ( -7.424621202458789426, 7.424621202458724589, 18.00000000000001421 ) ) ;
#2468 = EDGE_LOOP ( 'NONE', ( #78, #6017, #4100, #7426 ) ) ;
#2469 = CARTESIAN_POINT ( 'NONE',  ( -4.743843029824828861, 13.17239914596749450, 50.42453085894499765 ) ) ;
#2470 = LINE ( 'NONE', #5570, #8453 ) ;
#2471 = CARTESIAN_POINT ( 'NONE',  ( 1.837501619626329630, -16.30827793483733501, 15.64285714285714235 ) ) ;
#2472 = CARTESIAN_POINT ( 'NONE',  ( -1.967016585148659846, 16.29368510291087091, 32.63881657323070584 ) ) ;
#2473 = CARTESIAN_POINT ( 'NONE',  ( -9.837026868206066865, 5.012215536711416064, 11.84999999999997478 ) ) ;
#2474 = CARTESIAN_POINT ( 'NONE',  ( 9.355568503977840678, 4.766900247265305701, 3.899999999999959055 ) ) ;
#2475 = CARTESIAN_POINT ( 'NONE',  ( 14.00000000000000533, 0.000000000000000000, 0.000000000000000000 ) ) ;
#2476 = CARTESIAN_POINT ( 'NONE',  ( -55.00000000000002132, 0.000000000000000000, 0.000000000000000000 ) ) ;
#2477 = VECTOR ( 'NONE', #8016, 1000.000000000000000 ) ;
#2478 = ORIENTED_EDGE ( 'NONE', *, *, #2974, .F. ) ;
#2479 = CARTESIAN_POINT ( 'NONE',  ( -13.25633410266679313, 4.503970704919840529, 19.56738800180213644 ) ) ;
#2480 = CARTESIAN_POINT ( 'NONE',  ( 10.90442828429184274, 1.727091770866679310, 16.04999999999995808 ) ) ;
#2481 = CARTESIAN_POINT ( 'NONE',  ( -5.420364854931999155, -15.49051278174644253, 16.07142857142857650 ) ) ;
#2482 = CARTESIAN_POINT ( 'NONE',  ( -163.5680690899785930, 0.8268589710946947502, 12.97398861359800115 ) ) ;
#2483 = CARTESIAN_POINT ( 'NONE',  ( -4.743843029824828861, 13.17239914596749450, 44.42453085894499765 ) ) ;
#2484 = CARTESIAN_POINT ( 'NONE',  ( 7.842167650704563897, 7.771249796623202144, 5.751137918078548239 ) ) ;
#2486 = AXIS2_PLACEMENT_3D ( 'NONE', #1637, #10163, #4736 ) ;
#2485 = CARTESIAN_POINT ( 'NONE',  ( -7.098671581784199880, -7.027753727702804376, 10.25113791807858021 ) ) ;
#2487 = CIRCLE ( 'NONE', #1507, 0.9906000000000003691 ) ;
#2488 = AXIS2_PLACEMENT_3D ( 'NONE', #8057, #7287, #3931 ) ;
#2489 = CARTESIAN_POINT ( 'NONE',  ( 0.000000000000000000, 4.163799117101000559E-16, -3.299999999999999822 ) ) ;
#2490 = CARTESIAN_POINT ( 'NONE',  ( -7.556039541191334585, -11.78653521626503320, 8.289754855340721207 ) ) ;
#2491 = FILL_AREA_STYLE ('',( #7000 ) ) ;
#2492 = CARTESIAN_POINT ( 'NONE',  ( 9.809645194534072132, -9.989344678689256796, 13.00404056962644006 ) ) ;
#2493 = VERTEX_POINT ( 'NONE', #5898 ) ;
#2494 = AXIS2_PLACEMENT_3D ( 'NONE', #5346, #6877, #8603 ) ;
#2495 = LINE ( 'NONE', #8021, #1114 ) ;
#2496 = AXIS2_PLACEMENT_3D ( 'NONE', #9083, #5094, #6626 ) ;
#2497 = CARTESIAN_POINT ( 'NONE',  ( -11.60466159355861926, -11.60466159355875249, 46.50000000000002132 ) ) ;
#2498 = CARTESIAN_POINT ( 'NONE',  ( -158.0000000000000284, -6.938893903907228378E-15, 0.000000000000000000 ) ) ;
#2499 = CARTESIAN_POINT ( 'NONE',  ( -166.7173525949050088, -1.323475700837307700, 14.94282300546550069 ) ) ;
#2500 = CARTESIAN_POINT ( 'NONE',  ( 8.900167166472154889, -4.534861676072213577, 16.35000000000000497 ) ) ;
#2501 = CARTESIAN_POINT ( 'NONE',  ( 8.900167166472154889, -4.534861676072210024, 10.35000000000002274 ) ) ;
#2502 = DIRECTION ( 'NONE',  ( 0.000000000000000000, -6.338944243255235518E-49, 1.000000000000000000 ) ) ;
#2503 = CARTESIAN_POINT ( 'NONE',  ( -13.61519076058348254, -8.404922754268771001, 26.71832628391215536 ) ) ;
#2504 = AXIS2_PLACEMENT_3D ( 'NONE', #2298, #2959, #5442 ) ;
#2505 = DIRECTION ( 'NONE',  ( 0.000000000000000000, 1.000000000000000000, 0.000000000000000000 ) ) ;
#2506 = CARTESIAN_POINT ( 'NONE',  ( 11.22385875690717683, -11.40355824106234373, 37.00404056962644006 ) ) ;
#2507 = EDGE_LOOP ( 'NONE', ( #9847, #7329 ) ) ;
#2508 = CARTESIAN_POINT ( 'NONE',  ( -8.731428362939189114, 13.89598863503036341, 30.21428571428572596 ) ) ;
#2509 = CARTESIAN_POINT ( 'NONE',  ( 1.595359904487381852, 14.39304130769396828, -1.488941479308433177E-16 ) ) ;
#2510 = FACE_OUTER_BOUND ( 'NONE', #6282, .T. ) ;
#2511 = SURFACE_STYLE_USAGE ( .BOTH. , #917 ) ;
#2512 = FILL_AREA_STYLE ('',( #5512 ) ) ;
#2513 = CARTESIAN_POINT ( 'NONE',  ( 9.858066664633883036, 1.612135949262857082, 11.04886208192144359 ) ) ;
#2514 = CARTESIAN_POINT ( 'NONE',  ( -4.579542530753125895, 8.877401133907090625, 1.148862081921408151 ) ) ;
#2515 = CARTESIAN_POINT ( 'NONE',  ( 7.556039541191335474, 11.78653521626503320, 41.28975485534072476 ) ) ;
#2516 = CARTESIAN_POINT ( 'NONE',  ( -11.60466159355861926, -11.60466159355875249, 22.50000000000000000 ) ) ;
#2517 = CARTESIAN_POINT ( 'NONE',  ( -9.899494936611716867, 9.899494936611610285, 42.00000000000000000 ) ) ;
#2518 = CARTESIAN_POINT ( 'NONE',  ( 7.556039541191335474, 11.78653521626503320, 47.28975485534072476 ) ) ;
#2519 = CARTESIAN_POINT ( 'NONE',  ( 4.742819248065503146, 13.55419868402813677, 13.07142857142857295 ) ) ;
#2520 = CARTESIAN_POINT ( 'NONE',  ( -15.44569104238500046, -1.018491042384999545, 1.237085481564325490E-63 ) ) ;
#2521 = CARTESIAN_POINT ( 'NONE',  ( 9.333916720356675967, 4.809394265263123636, 4.898862081921403266 ) ) ;
#2522 = ORIENTED_EDGE ( 'NONE', *, *, #7750, .T. ) ;
#2523 = CARTESIAN_POINT ( 'NONE',  ( 7.340858601237956194, 11.92174236212700045, 51.28167371608785174 ) ) ;
#2524 = VERTEX_POINT ( 'NONE', #9898 ) ;
#2525 = DIRECTION ( 'NONE',  ( 0.000000000000000000, 6.938893903907220674E-18, 1.000000000000000000 ) ) ;
#2526 = CARTESIAN_POINT ( 'NONE',  ( -13.89598863503045933, 8.731428362939027465, 23.78571428571429180 ) ) ;
#2527 = VECTOR ( 'NONE', #6510, 1000.000000000000000 ) ;
#2528 = CARTESIAN_POINT ( 'NONE',  ( -15.44746603149413922, -5.543385399275820191, 30.92453085894499765 ) ) ;
#2529 = CARTESIAN_POINT ( 'NONE',  ( -5.012215536711506658, 9.837026868206022456, 6.149999999999980815 ) ) ;
#2530 = CARTESIAN_POINT ( 'NONE',  ( 10.37072757624895836, -1.642561882922355609, 7.199999999999984190 ) ) ;
#2531 = DIRECTION ( 'NONE',  ( 0.000000000000000000, 6.338944243255235518E-49, -1.000000000000000000 ) ) ;
#2532 = ORIENTED_EDGE ( 'NONE', *, *, #8210, .F. ) ;
#2533 = CARTESIAN_POINT ( 'NONE',  ( -1.737328882695368115, 14.25515036105620581, 20.63881657323070939 ) ) ;
#2534 = CARTESIAN_POINT ( 'NONE',  ( -1.727091770866549414, -10.90442828429184807, 13.95000000000002416 ) ) ;
#2535 = EDGE_CURVE ( 'NONE', #2905, #166, #5283, .T. ) ;
#2536 = DIRECTION ( 'NONE',  ( 1.000000000000000000, 4.755747939841215952E-17, -0.000000000000000000 ) ) ;
#2537 = EDGE_CURVE ( 'NONE', #594, #9409, #5452, .T. ) ;
#2538 = CARTESIAN_POINT ( 'NONE',  ( -12.22833218042443271, 7.529642458189139909, 43.78167371608784464 ) ) ;
#2539 = CARTESIAN_POINT ( 'NONE',  ( -1.776620879821455556, -10.89658364409025637, 12.95113791807858128 ) ) ;
#2540 = CARTESIAN_POINT ( 'NONE',  ( -1.612135949262737844, -9.858066664633888365, 12.95113791807858128 ) ) ;
#2541 = EDGE_CURVE ( 'NONE', #3552, #7029, #2645, .T. ) ;
#2542 = AXIS2_PLACEMENT_3D ( 'NONE', #1616, #4613, #6093 ) ;
#2543 = DIRECTION ( 'NONE',  ( 0.000000000000000000, -6.338944243255235518E-49, 1.000000000000000000 ) ) ;
#2544 = CARTESIAN_POINT ( 'NONE',  ( 1.478298951650704351, -14.28433602490913579, 13.64689771248357708 ) ) ;
#2545 =( NAMED_UNIT ( * ) PLANE_ANGLE_UNIT ( ) SI_UNIT ( $, .RADIAN. ) );
#2546 = CARTESIAN_POINT ( 'NONE',  ( 7.529642458189280241, -12.22833218042435099, 13.21832628391215181 ) ) ;
#2547 = EDGE_LOOP ( 'NONE', ( #3091, #8288 ) ) ;
#2548 = CARTESIAN_POINT ( 'NONE',  ( 9.899494936611612061, 9.899494936611718643, 49.50000000000000000 ) ) ;
#2549 = CARTESIAN_POINT ( 'NONE',  ( 1.665163862719847732, 15.91362231745477374, 14.85310228751642470 ) ) ;
#2550 = DIRECTION ( 'NONE',  ( 0.000000000000000000, 0.000000000000000000, 1.000000000000000000 ) ) ;
#2551 = CARTESIAN_POINT ( 'NONE',  ( -165.1406648078596220, -2.150094845865166082, 14.84510330590739180 ) ) ;
#2552 = CARTESIAN_POINT ( 'NONE',  ( -7.098671581784199880, -7.027753727702804376, 1.251137918078559563 ) ) ;
#2553 = CARTESIAN_POINT ( 'NONE',  ( 1.486127417882244783, -9.383039235653791721, 4.800000000000026468 ) ) ;
#2554 = CARTESIAN_POINT ( 'NONE',  ( -108.0000000000000284, 0.000000000000000000, 0.000000000000000000 ) ) ;
#2555 = CARTESIAN_POINT ( 'NONE',  ( 15.53355953199861794, 5.297344310588528060, 23.93261199819786711 ) ) ;
#2556 = CARTESIAN_POINT ( 'NONE',  ( 13.21436662431716869, -4.623906867372263640, 32.57142857142856940 ) ) ;
#2557 = CARTESIAN_POINT ( 'NONE',  ( -16.29368510291090288, 1.967016585148476215, 27.36118342676929416 ) ) ;
#2558 = ORIENTED_EDGE ( 'NONE', *, *, #6528, .T. ) ;
#2559 = CARTESIAN_POINT ( 'NONE',  ( 1.837501619626330074, -16.30827793483733501, 27.64285714285714590 ) ) ;
#2560 = CARTESIAN_POINT ( 'NONE',  ( -4.309600312599306982, 13.44913272913615465, 3.300085072504084867E-16 ) ) ;
#2561 = CARTESIAN_POINT ( 'NONE',  ( 13.89598863503046111, -8.731428362939032795, 14.78571428571429358 ) ) ;
#2562 = APPLICATION_CONTEXT ( 'automotive_design' ) ;
#2563 = FILL_AREA_STYLE_COLOUR ( '', #2962 ) ;
#2564 = EDGE_CURVE ( 'NONE', #3839, #9051, #9098, .T. ) ;
#2565 = DIRECTION ( 'NONE',  ( 0.000000000000000000, -6.338944243255235518E-49, 1.000000000000000000 ) ) ;
#2566 = CARTESIAN_POINT ( 'NONE',  ( -7.458344646081709328, 7.390897758835805575, 15.99886208192142512 ) ) ;
#2567 = CARTESIAN_POINT ( 'NONE',  ( -1.478298951650703019, 14.28433602490913579, 46.64689771248358596 ) ) ;
#2568 = CARTESIAN_POINT ( 'NONE',  ( 8.512513224245308763, 13.54758718765259040, 13.28571428571429003 ) ) ;
#2569 = SURFACE_SIDE_STYLE ('',( #6482 ) ) ;
#2570 = CARTESIAN_POINT ( 'NONE',  ( -13.59724543428031573, -4.619798703722008959, 38.93261199819787777 ) ) ;
#2571 = CARTESIAN_POINT ( 'NONE',  ( -9.899494936611716867, 9.899494936611610285, 11.99999999999999645 ) ) ;
#2572 = CARTESIAN_POINT ( 'NONE',  ( -8.900167166472160218, 4.534861676072232228, 14.84999999999999609 ) ) ;
#2573 = CARTESIAN_POINT ( 'NONE',  ( 10.37818827243067510, -1.595456901104499448, 11.19886208192145816 ) ) ;
#2574 = ORIENTED_EDGE ( 'NONE', *, *, #4434, .T. ) ;
#2575 = CARTESIAN_POINT ( 'NONE',  ( -13.55419868402807992, -4.742819248065651472, 4.928571428571430602 ) ) ;
#2576 = EDGE_LOOP ( 'NONE', ( #7299, #6905, #10175, #9434 ) ) ;
#2577 = FACE_OUTER_BOUND ( 'NONE', #6322, .T. ) ;
#2578 = CARTESIAN_POINT ( 'NONE',  ( 5.284464991282756152, -15.10213328493384743, 15.42857142857143060 ) ) ;
#2579 = ADVANCED_FACE ( 'NONE', ( #5084 ), #8235, .T. ) ;
#2580 = CARTESIAN_POINT ( 'NONE',  ( -15.14410076328353227, 5.164528828830164287, 37.56738800180213644 ) ) ;
#2581 = CARTESIAN_POINT ( 'NONE',  ( -9.355568503977838901, -4.766900247265279944, 5.400000000000016342 ) ) ;
#2582 = CARTESIAN_POINT ( 'NONE',  ( -10.37072757624895836, 1.642561882922380923, 17.69999999999999218 ) ) ;
#2583 = CARTESIAN_POINT ( 'NONE',  ( 13.55419868402807992, 4.742819248065649695, 13.92857142857143060 ) ) ;
#2584 = ORIENTED_EDGE ( 'NONE', *, *, #9584, .F. ) ;
#2585 = CARTESIAN_POINT ( 'NONE',  ( 9.837026868206070418, -5.012215536711395636, 16.35000000000000853 ) ) ;
#2586 = DIRECTION ( 'NONE',  ( -1.000000000000000000, 0.000000000000000000, 0.000000000000000000 ) ) ;
#2587 = CARTESIAN_POINT ( 'NONE',  ( -12.22833218042443271, 7.529642458189139909, 37.78167371608785174 ) ) ;
#2588 = CARTESIAN_POINT ( 'NONE',  ( -7.390897758835869524, 7.458344646081637386, 11.00113791807855002 ) ) ;
#2589 = CARTESIAN_POINT ( 'NONE',  ( -4.967534682030703586, 9.859792900771061852, 8.151137918078559252 ) ) ;
#2590 = STYLED_ITEM ( 'NONE', ( #2064 ), #3605 ) ;
#2591 = DIRECTION ( 'NONE',  ( 0.000000000000000000, 0.000000000000000000, 1.000000000000000000 ) ) ;
#2592 = CARTESIAN_POINT ( 'NONE',  ( 13.92619789766827587, 1.441234910513398582, 24.14689771248357530 ) ) ;
#2593 = CARTESIAN_POINT ( 'NONE',  ( 1.478298951650704351, -14.28433602490913579, 19.64689771248358596 ) ) ;
#2595 = FACE_BOUND ( 'NONE', #7310, .T. ) ;
#2594 = TOROIDAL_SURFACE ( 'NONE', #8372, 2.200000000000001066, 0.2000000000000000111 ) ;
#2596 = CARTESIAN_POINT ( 'NONE',  ( -13.47998361472151174, -8.620103694222146729, 6.710245144659284122 ) ) ;
#2597 = DIRECTION ( 'NONE',  ( 0.000000000000000000, 0.000000000000000000, 1.000000000000000000 ) ) ;
#2598 = LINE ( 'NONE', #3472, #5924 ) ;
#2599 = CARTESIAN_POINT ( 'NONE',  ( 6.683790977649321619, -6.751237864895082375, 3.501137918078585987 ) ) ;
#2600 = CARTESIAN_POINT ( 'NONE',  ( -8.464561979789474222, -4.312909747525729642, 2.400000000000013234 ) ) ;
#2601 = DIRECTION ( 'NONE',  ( 0.7071067811865510144, -0.7071067811865440200, 0.000000000000000000 ) ) ;
#2602 = CARTESIAN_POINT ( 'NONE',  ( -13.82664651025767100, 8.841785722321537477, 39.78975485534073186 ) ) ;
#2603 = CARTESIAN_POINT ( 'NONE',  ( 7.639999817571789364, -12.15899005565156266, 33.21428571428571530 ) ) ;
#2604 = CARTESIAN_POINT ( 'NONE',  ( 13.61519076058348254, 8.404922754268771001, 41.71832628391215536 ) ) ;
#2605 = ORIENTED_EDGE ( 'NONE', *, *, #2801, .F. ) ;
#2606 = CARTESIAN_POINT ( 'NONE',  ( 8.731428362939190890, -13.89598863503036164, 27.21428571428572241 ) ) ;
#2607 = CARTESIAN_POINT ( 'NONE',  ( -7.292276458266168326, 11.99875552204202833, 2.357314452189448168E-16 ) ) ;
#2608 = CARTESIAN_POINT ( 'NONE',  ( 1.791431617652837316, 15.89939535829188877, 18.85714285714285765 ) ) ;
#2609 = CARTESIAN_POINT ( 'NONE',  ( 4.534861676072320158, -8.900167166472098046, 1.650000000000006128 ) ) ;
#2610 = CARTESIAN_POINT ( 'NONE',  ( 4.724406229267374968, 9.377220287599064008, 16.59886208192139989 ) ) ;
#2611 = PRODUCT_DEFINITION_FORMATION_WITH_SPECIFIED_SOURCE ( 'ANY', '', #6639, .NOT_KNOWN. ) ;
#2612 = CARTESIAN_POINT ( 'NONE',  ( 5.164528828830335705, -15.14410076328347543, 13.43261199819786711 ) ) ;
#2613 = CARTESIAN_POINT ( 'NONE',  ( -11.60466159355861926, -11.60466159355875249, 34.50000000000000000 ) ) ;
#2614 = CARTESIAN_POINT ( 'NONE',  ( -13.21436662431716869, 4.623906867372262752, 47.57142857142857650 ) ) ;
#2615 = CARTESIAN_POINT ( 'NONE',  ( -15.06016580658428694, 5.404401153735006957, 9.575469141055007682 ) ) ;
#2616 = CARTESIAN_POINT ( 'NONE',  ( -13.91197093850538380, -1.567502665446387278, 11.14285714285714235 ) ) ;
#2617 = DIRECTION ( 'NONE',  ( -1.000000000000000000, 0.000000000000000000, 0.000000000000000000 ) ) ;
#2618 = CARTESIAN_POINT ( 'NONE',  ( -5.056896391392315948, 9.814260835640997271, 7.148862081921437017 ) ) ;
#2619 = ORIENTED_EDGE ( 'NONE', *, *, #863, .F. ) ;
#2620 = CARTESIAN_POINT ( 'NONE',  ( -4.742819248065502258, -13.55419868402813677, 10.07142857142856940 ) ) ;
#2621 = ORIENTED_EDGE ( 'NONE', *, *, #8540, .F. ) ;
#2622 = CARTESIAN_POINT ( 'NONE',  ( 15.10213328493390783, -5.284464991282587398, 26.57142857142857295 ) ) ;
#2623 = CARTESIAN_POINT ( 'NONE',  ( 15.44746603149413922, 5.543385399275817527, 33.92453085894499054 ) ) ;
#2624 = CARTESIAN_POINT ( 'NONE',  ( -1.727091770866549414, -10.90442828429185695, 4.950000000000017053 ) ) ;
#2625 = CARTESIAN_POINT ( 'NONE',  ( 5.012215536711511987, -9.837026868205999364, 16.64999999999999858 ) ) ;
#2626 = CARTESIAN_POINT ( 'NONE',  ( -7.448449071214644945, -11.85413878919601771, 16.28571428571428470 ) ) ;
#2627 = CARTESIAN_POINT ( 'NONE',  ( -1.737328882695368115, 14.25515036105620581, 32.63881657323070584 ) ) ;
#2628 = AXIS2_PLACEMENT_3D ( 'NONE', #6162, #6212, #9540 ) ;
#2629 = EDGE_LOOP ( 'NONE', ( #1297, #182, #3115, #7849 ) ) ;
#2630 = FACE_OUTER_BOUND ( 'NONE', #9178, .T. ) ;
#2631 = DIRECTION ( 'NONE',  ( -0.000000000000000000, 0.000000000000000000, -1.000000000000000000 ) ) ;
#2632 = CARTESIAN_POINT ( 'NONE',  ( -7.340858601237953529, -11.92174236212700222, 42.28167371608785174 ) ) ;
#2633 = CARTESIAN_POINT ( 'NONE',  ( 4.809394265263009061, 9.333916720356734587, 11.60113791807856742 ) ) ;
#2634 = CARTESIAN_POINT ( 'NONE',  ( 7.390897758835871301, -7.458344646081618734, 0.5011379180785839882 ) ) ;
#2635 = DIRECTION ( 'NONE',  ( 0.000000000000000000, -9.714451465470119729E-16, -1.000000000000000000 ) ) ;
#2636 = CARTESIAN_POINT ( 'NONE',  ( -4.503970704919988854, 13.25633410266674517, 16.43261199819786356 ) ) ;
#2637 = AXIS2_PLACEMENT_3D ( 'NONE', #6994, #3069, #2301 ) ;
#2638 = VECTOR ( 'NONE', #5736, 1000.000000000000000 ) ;
#2639 = CARTESIAN_POINT ( 'NONE',  ( -4.766900247265192014, -9.355568503977867323, 11.09999999999999787 ) ) ;
#2640 = CARTESIAN_POINT ( 'NONE',  ( 5.404401153735178376, -15.06016580658422477, 41.42453085894499765 ) ) ;
#2641 = DIRECTION ( 'NONE',  ( 0.000000000000000000, -6.338944243255235518E-49, 1.000000000000000000 ) ) ;
#2642 = CARTESIAN_POINT ( 'NONE',  ( -8.404922754268618235, -13.61519076058357491, 12.28167371608784997 ) ) ;
#2643 = DIRECTION ( 'NONE',  ( 1.000000000000000000, -4.575525868300071581E-16, -0.000000000000000000 ) ) ;
#2644 = CARTESIAN_POINT ( 'NONE',  ( -162.9064615436232373, -0.5639517720651365806, 14.99163496215254199 ) ) ;
#2645 = CIRCLE ( 'NONE', #10085, 17.72919999999999874 ) ;
#2646 = AXIS2_PLACEMENT_3D ( 'NONE', #1216, #6571, #9806 ) ;
#2647 = AXIS2_PLACEMENT_3D ( 'NONE', #3893, #590, #4517 ) ;
#2648 = CARTESIAN_POINT ( 'NONE',  ( 9.375578539472099848, -1.533232399699987702, 3.201137918078536426 ) ) ;
#2649 = CARTESIAN_POINT ( 'NONE',  ( 8.900167166472154889, -4.534861676072210912, 19.34999999999996945 ) ) ;
#2650 = CARTESIAN_POINT ( 'NONE',  ( -162.8500000000000227, 0.1404123523451087929, 14.99999999999999822 ) ) ;
#2651 = CARTESIAN_POINT ( 'NONE',  ( 8.621071003556677326, -13.96533075980314287, 37.21832628391215536 ) ) ;
#2652 = CARTESIAN_POINT ( 'NONE',  ( -12.15899005565164792, 7.639999817571651697, 35.78571428571429180 ) ) ;
#2653 = AXIS2_PLACEMENT_3D ( 'NONE', #3032, #6790, #2312 ) ;
#2654 = VECTOR ( 'NONE', #3460, 1000.000000000000000 ) ;
#2655 = VERTEX_POINT ( 'NONE', #7565 ) ;
#2656 = CARTESIAN_POINT ( 'NONE',  ( 13.89598863503046111, -8.731428362939032795, 26.78571428571429536 ) ) ;
#2657 = CARTESIAN_POINT ( 'NONE',  ( -108.0000000000000284, 0.000000000000000000, 0.000000000000000000 ) ) ;
#2658 = CARTESIAN_POINT ( 'NONE',  ( -13.89598863503046111, 8.731428362939027465, 11.78571428571428115 ) ) ;
#2659 = FACE_OUTER_BOUND ( 'NONE', #2071, .T. ) ;
#2660 = CARTESIAN_POINT ( 'NONE',  ( -1.513077731352923339, -9.873755945037078874, 17.94886208192144395 ) ) ;
#2661 = CARTESIAN_POINT ( 'NONE',  ( 1.513077731352925115, 9.873755945037103743, 7.448862081921427070 ) ) ;
#2662 = PRESENTATION_LAYER_ASSIGNMENT (  '', '', ( #7792 ) ) ;
#2663 = UNCERTAINTY_MEASURE_WITH_UNIT (LENGTH_MEASURE( 1.000000000000000082E-05 ), #102, 'distance_accuracy_value', 'NONE');
#2664 = CARTESIAN_POINT ( 'NONE',  ( -1.707986654103994528, 16.32287076676380266, 16.64689771248358596 ) ) ;
#2665 = CARTESIAN_POINT ( 'NONE',  ( -13.89598863503046111, 8.731428362939027465, 35.78571428571429180 ) ) ;
#2666 = CARTESIAN_POINT ( 'NONE',  ( 16.29368510291089223, -1.967016585148476882, 0.3611834267692887734 ) ) ;
#2667 = CIRCLE ( 'NONE', #8620, 18.00000000000000355 ) ;
#2668 = CARTESIAN_POINT ( 'NONE',  ( -9.899494936611716867, 9.899494936611610285, 5.999999999999998224 ) ) ;
#2669 = DIRECTION ( 'NONE',  ( 0.000000000000000000, 0.000000000000000000, 1.000000000000000000 ) ) ;
#2670 = CARTESIAN_POINT ( 'NONE',  ( -4.724406229267374968, -9.377220287599046245, 12.09886208192144252 ) ) ;
#2671 = ORIENTED_EDGE ( 'NONE', *, *, #4371, .F. ) ;
#2672 = CARTESIAN_POINT ( 'NONE',  ( 1.567502665446232957, 13.91197093850540156, 12.85714285714285943 ) ) ;
#2673 = EDGE_LOOP ( 'NONE', ( #1525, #2522, #201 ) ) ;
#2674 = CARTESIAN_POINT ( 'NONE',  ( 11.60466159355861926, 11.60466159355874716, 31.50000000000000711 ) ) ;
#2675 = CARTESIAN_POINT ( 'NONE',  ( 16.32287076676382043, -1.707986654103810897, 40.35310228751642825 ) ) ;
#2676 = CARTESIAN_POINT ( 'NONE',  ( 9.355568503977840678, 4.766900247265305701, 9.900000000000019895 ) ) ;
#2677 = CARTESIAN_POINT ( 'NONE',  ( 7.639999817571788476, -12.15899005565156266, 9.214285714285717077 ) ) ;
#2678 = ORIENTED_EDGE ( 'NONE', *, *, #5440, .F. ) ;
#2679 = EDGE_CURVE ( 'NONE', #4852, #94, #1162, .T. ) ;
#2680 = CARTESIAN_POINT ( 'NONE',  ( 7.750357176954296712, -12.08964793087877787, 29.21024514465927879 ) ) ;
#2681 = CYLINDRICAL_SURFACE ( 'NONE', #7208, 18.00000000000000355 ) ;
#2682 = CIRCLE ( 'NONE', #6305, 8.000000000000000000 ) ;
#2683 = CARTESIAN_POINT ( 'NONE',  ( 3.002363214934308022, 13.70813944144856755, 48.73000000000003240 ) ) ;
#2684 = EDGE_CURVE ( 'NONE', #1705, #6462, #3540, .T. ) ;
#2685 = CARTESIAN_POINT ( 'NONE',  ( -14.28433602490915000, 1.478298951650542481, 37.35310228751641404 ) ) ;
#2686 = CARTESIAN_POINT ( 'NONE',  ( -9.814260835641038128, 5.056896391392221801, 13.85113791807855321 ) ) ;
#2687 = CARTESIAN_POINT ( 'NONE',  ( -1.776620879821455556, -10.89658364409025637, 6.951137918078597266 ) ) ;
#2688 = AXIS2_PLACEMENT_3D ( 'NONE', #7784, #754, #70 ) ;
#2689 = CARTESIAN_POINT ( 'NONE',  ( 9.511495879682431411E-16, -20.00000000000000000, 2.449293598294706513E-15 ) ) ;
#2690 = CARTESIAN_POINT ( 'NONE',  ( 4.503970704919991519, -13.25633410266674517, 19.43261199819785645 ) ) ;
#2691 = PRODUCT_DEFINITION_SHAPE ( 'NONE', 'NONE',  #10231 ) ;
#2692 = CARTESIAN_POINT ( 'NONE',  ( 12.08964793087886314, -7.750357176954162597, 24.78975485534072476 ) ) ;
#2693 = CARTESIAN_POINT ( 'NONE',  ( 9.355568503977840678, 4.766900247265305701, 3.899999999999959055 ) ) ;
#2694 = CARTESIAN_POINT ( 'NONE',  ( -5.297344310588352201, -15.53355953199867301, 42.06738800180214355 ) ) ;
#2695 = CARTESIAN_POINT ( 'NONE',  ( -168.0000000000000284, 13.00000000000000178, 0.000000000000000000 ) ) ;
#2696 = CARTESIAN_POINT ( 'NONE',  ( 16.30827793483735633, -1.837501619626142890, 20.35714285714286476 ) ) ;
#2697 = CARTESIAN_POINT ( 'NONE',  ( 11.40355824106246985, -11.22385875690704538, 4.995959430373563492 ) ) ;
#2698 = DIRECTION ( 'NONE',  ( 0.000000000000000000, 6.938893903907221444E-18, 1.000000000000000000 ) ) ;
#2699 = EDGE_CURVE ( 'NONE', #5232, #8643, #1211, .T. ) ;
#2700 = CARTESIAN_POINT ( 'NONE',  ( 1.612135949262739398, 9.858066664633913234, 5.451137918078557298 ) ) ;
#2701 = CARTESIAN_POINT ( 'NONE',  ( 7.098671581784200768, 7.027753727702831021, -0.2488620819214366897 ) ) ;
#2702 = DIRECTION ( 'NONE',  ( -0.000000000000000000, -0.000000000000000000, -1.000000000000000000 ) ) ;
#2703 = CARTESIAN_POINT ( 'NONE',  ( -11.85413878919593422, -7.448449071214776396, 28.71428571428571530 ) ) ;
#2704 = CARTESIAN_POINT ( 'NONE',  ( -10.15407889436378852, -10.15407889436390576, 40.50000000000000711 ) ) ;
#2705 = ORIENTED_EDGE ( 'NONE', *, *, #2060, .F. ) ;
#2706 = CARTESIAN_POINT ( 'NONE',  ( -1.967016585148659846, 16.29368510291087091, 2.638816573230710727 ) ) ;
#2707 = CARTESIAN_POINT ( 'NONE',  ( -1.373322081274849449, 15.69029061493039023, 5.081489463560647903E-16 ) ) ;
#2708 = CARTESIAN_POINT ( 'NONE',  ( 16.30827793483735633, -1.837501619626142890, 20.35714285714286476 ) ) ;
#2709 = CARTESIAN_POINT ( 'NONE',  ( -4.270415729527831772, -8.486213763410670907, 18.09886208192144252 ) ) ;
#2710 = CARTESIAN_POINT ( 'NONE',  ( -9.858066664633883036, -1.612135949262831547, 6.548862081921412504 ) ) ;
#2711 = CARTESIAN_POINT ( 'NONE',  ( -15.06016580658428694, 5.404401153735006957, 9.575469141055007682 ) ) ;
#2712 = CARTESIAN_POINT ( 'NONE',  ( 5.284464991282756152, -15.10213328493384743, 33.42857142857143060 ) ) ;
#2713 = CARTESIAN_POINT ( 'NONE',  ( -12.15899005565164792, 7.639999817571650809, 47.78571428571429891 ) ) ;
#2714 = CARTESIAN_POINT ( 'NONE',  ( -15.91362231745475597, -1.665163862720028254, 3.146897712483577969 ) ) ;
#2715 = CARTESIAN_POINT ( 'NONE',  ( -1.607813917173034124, 14.26974319298267524, 18.64285714285715656 ) ) ;
#2716 = CARTESIAN_POINT ( 'NONE',  ( -5.420364854931999155, -15.49051278174644253, 10.07142857142856940 ) ) ;
#2717 = CARTESIAN_POINT ( 'NONE',  ( -10.89658364409024749, -1.776620879821561472, 9.548862081921404510 ) ) ;
#2718 = ORIENTED_EDGE ( 'NONE', *, *, #1660, .T. ) ;
#2719 = CARTESIAN_POINT ( 'NONE',  ( 14.26974319298268767, -1.607813917172876916, 14.35714285714285587 ) ) ;
#2720 = EDGE_CURVE ( 'NONE', #8149, #999, #7043, .T. ) ;
#2721 = ORIENTED_EDGE ( 'NONE', *, *, #8828, .F. ) ;
#2722 = CARTESIAN_POINT ( 'NONE',  ( 1.791431617652837316, 15.89939535829188877, 24.85714285714285765 ) ) ;
#2723 = CARTESIAN_POINT ( 'NONE',  ( 12.22833218042443271, -7.529642458189144349, 4.781673716087850856 ) ) ;
#2724 = CARTESIAN_POINT ( 'NONE',  ( -9.837026868206066865, 5.012215536711416064, 17.85000000000001918 ) ) ;
#2725 = PRODUCT_CONTEXT ( 'NONE', #5533, 'mechanical' ) ;
#2726 = CARTESIAN_POINT ( 'NONE',  ( -13.55419868402807992, -4.742819248065651472, 16.92857142857143060 ) ) ;
#2727 = CARTESIAN_POINT ( 'NONE',  ( 7.340858601237956194, 11.92174236212700045, 33.28167371608784464 ) ) ;
#2728 = SURFACE_STYLE_FILL_AREA ( #9781 ) ;
#2729 = CARTESIAN_POINT ( 'NONE',  ( -4.169902070941136074, -13.58603705635637482, -1.270000000000007123 ) ) ;
#2730 = CARTESIAN_POINT ( 'NONE',  ( -6.751237864895158758, 6.683790977649255005, 3.998862081921419342 ) ) ;
#2731 = CARTESIAN_POINT ( 'NONE',  ( 4.742819248065503146, 13.55419868402813677, 1.071428571428570287 ) ) ;
#2732 = CARTESIAN_POINT ( 'NONE',  ( -10.36326688006724162, 1.689666864740235308, 16.70113791807854398 ) ) ;
#2733 = CARTESIAN_POINT ( 'NONE',  ( 10.36326688006723984, -1.689666864740210883, 6.201137918078538647 ) ) ;
#2734 = FACE_OUTER_BOUND ( 'NONE', #1438, .T. ) ;
#2735 = CARTESIAN_POINT ( 'NONE',  ( -13.92619789766827054, -1.441234910513399470, 21.14689771248358241 ) ) ;
#2736 =( NAMED_UNIT ( * ) SI_UNIT ( $, .STERADIAN. ) SOLID_ANGLE_UNIT ( ) );
#2737 = CARTESIAN_POINT ( 'NONE',  ( -13.59724543428031573, -4.619798703722008959, 20.93261199819787066 ) ) ;
#2738 = CARTESIAN_POINT ( 'NONE',  ( 1.727091770866550968, 10.90442828429187294, 12.44999999999995666 ) ) ;
#2739 = CARTESIAN_POINT ( 'NONE',  ( 15.88516839912898071, 1.917699372586004092, 40.13881657323070584 ) ) ;
#2740 = CARTESIAN_POINT ( 'NONE',  ( -8.334518847312166301, 13.50009031046634611, 48.72999999999998977 ) ) ;
#2741 = CARTESIAN_POINT ( 'NONE',  ( -163.3939431418218646, -0.4350255360096275670, 12.99423751676100558 ) ) ;
#2742 = AXIS2_PLACEMENT_3D ( 'NONE', #7490, #8319, #5061 ) ;
#2743 = EDGE_CURVE ( 'NONE', #9801, #5925, #4462, .T. ) ;
#2744 = CARTESIAN_POINT ( 'NONE',  ( -9.873755945037078874, -1.513077731353020594, 7.551137918078578259 ) ) ;
#2745 = CARTESIAN_POINT ( 'NONE',  ( -1.562606840307830591, -9.865911304835478290, 16.94999999999998863 ) ) ;
#2746 = CARTESIAN_POINT ( 'NONE',  ( -163.6887781248447880, 1.709617356372435948, 14.90246111853683608 ) ) ;
#2747 =( REPRESENTATION_RELATIONSHIP ('NONE','NONE', #58, #5586 ) REPRESENTATION_RELATIONSHIP_WITH_TRANSFORMATION ( #9404 )SHAPE_REPRESENTATION_RELATIONSHIP( ) );
#2748 = CARTESIAN_POINT ( 'NONE',  ( 9.899494936611718643, -9.899494936611608509, 27.00000000000000355 ) ) ;
#2749 = MECHANICAL_DESIGN_GEOMETRIC_PRESENTATION_REPRESENTATION (  '', ( #116 ), #3578 ) ;
#2750 = CARTESIAN_POINT ( 'NONE',  ( -13.21436662431716869, 4.623906867372262752, 35.57142857142857650 ) ) ;
#2751 = VERTEX_POINT ( 'NONE', #3851 ) ;
#2752 = CARTESIAN_POINT ( 'NONE',  ( 5.284464991282756152, -15.10213328493384743, 39.42857142857143060 ) ) ;
#2753 = DIRECTION ( 'NONE',  ( -4.755747939841215952E-17, 1.000000000000000000, 0.000000000000000000 ) ) ;
#2754 = CARTESIAN_POINT ( 'NONE',  ( -5.284464991282755264, 15.10213328493384743, 18.42857142857143415 ) ) ;
#2755 = DIRECTION ( 'NONE',  ( -0.000000000000000000, 0.000000000000000000, -1.000000000000000000 ) ) ;
#2756 = CARTESIAN_POINT ( 'NONE',  ( 9.390499931835536884, -1.439022436064273158, 14.19886208192146171 ) ) ;
#2757 = CARTESIAN_POINT ( 'NONE',  ( -9.390499931835536884, 1.439022436064298249, 3.698862081921452827 ) ) ;
#2758 = CARTESIAN_POINT ( 'NONE',  ( -15.53355953199861794, -5.297344310588530725, 8.932611998197868886 ) ) ;
#2759 = CARTESIAN_POINT ( 'NONE',  ( 8.512513224245308763, 13.54758718765259040, 31.28571428571428470 ) ) ;
#2760 = CARTESIAN_POINT ( 'NONE',  ( -1.567502665446231180, -13.91197093850540334, 45.85714285714286120 ) ) ;
#2761 = AXIS2_PLACEMENT_3D ( 'NONE', #3189, #8465, #4641 ) ;
#2762 = CARTESIAN_POINT ( 'NONE',  ( 13.61519076058348254, 8.404922754268771001, 11.71832628391215181 ) ) ;
#2763 = CARTESIAN_POINT ( 'NONE',  ( -7.639999817571787588, 12.15899005565156266, 30.21428571428572596 ) ) ;
#2764 = CARTESIAN_POINT ( 'NONE',  ( -5.284464991282755264, 15.10213328493384743, 0.4285714285714309346 ) ) ;
#2765 = CARTESIAN_POINT ( 'NONE',  ( 1.837501619626330074, -16.30827793483733501, 45.64285714285716011 ) ) ;
#2766 = ORIENTED_EDGE ( 'NONE', *, *, #4241, .T. ) ;
#2767 = CARTESIAN_POINT ( 'NONE',  ( 1.607813917173038121, -14.26974319298267346, 15.64285714285714235 ) ) ;
#2768 = VERTEX_POINT ( 'NONE', #3014 ) ;
#2769 = ADVANCED_BREP_SHAPE_REPRESENTATION ( '', ( #7008, #3995 ), #7950 ) ;
#2770 = CARTESIAN_POINT ( 'NONE',  ( 8.512513224245308763, 13.54758718765259040, 37.28571428571429180 ) ) ;
#2771 = CARTESIAN_POINT ( 'NONE',  ( 16.32287076676382043, -1.707986654103810897, 46.35310228751641404 ) ) ;
#2772 = CARTESIAN_POINT ( 'NONE',  ( -7.458344646081709328, 7.390897758835799358, 3.998862081921419342 ) ) ;
#2773 = PRODUCT ( 'BR-105', 'BR-105', '', ( #9249 ) ) ;
#2774 = PRODUCT_CONTEXT ( 'NONE', #5395, 'mechanical' ) ;
#2775 = CARTESIAN_POINT ( 'NONE',  ( -12.15899005565164792, 7.639999817571650809, 11.78571428571428292 ) ) ;
#2776 = ORIENTED_EDGE ( 'NONE', *, *, #7726, .F. ) ;
#2777 = ORIENTED_EDGE ( 'NONE', *, *, #6679, .T. ) ;
#2778 = CARTESIAN_POINT ( 'NONE',  ( -4.743843029824828861, 13.17239914596749450, 32.42453085894499054 ) ) ;
#2779 = CARTESIAN_POINT ( 'NONE',  ( 9.449716478673138909, 10.73265495317049023, 48.73000000000004661 ) ) ;
#2780 = CARTESIAN_POINT ( 'NONE',  ( 9.333916720356675967, 4.809394265263123636, 19.89886208192141481 ) ) ;
#2781 = EDGE_CURVE ( 'NONE', #9967, #8413, #8938, .T. ) ;
#2782 = CARTESIAN_POINT ( 'NONE',  ( -1.642561882922479732, 10.37072757624895303, 3.299999999999969624 ) ) ;
#2783 = CARTESIAN_POINT ( 'NONE',  ( 1.595456901104624459, -10.37818827243064490, 6.801137918078597799 ) ) ;
#2784 = CARTESIAN_POINT ( 'NONE',  ( 0.000000000000000000, 0.000000000000000000, 0.000000000000000000 ) ) ;
#2785 = DIRECTION ( 'NONE',  ( 0.000000000000000000, 0.000000000000000000, 1.000000000000000000 ) ) ;
#2786 = CARTESIAN_POINT ( 'NONE',  ( -10.37072757624895836, 1.642561882922380034, 11.69999999999998863 ) ) ;
#2787 = CARTESIAN_POINT ( 'NONE',  ( -8.841785722321695573, 13.82664651025757152, 44.21024514465928235 ) ) ;
#2788 = ORIENTED_EDGE ( 'NONE', *, *, #6539, .T. ) ;
#2789 = CARTESIAN_POINT ( 'NONE',  ( -5.498463549856485777, 12.96445134456831383, 48.73000000000003951 ) ) ;
#2790 = CARTESIAN_POINT ( 'NONE',  ( 1.791431617652837316, 15.89939535829188877, 18.85714285714285765 ) ) ;
#2791 = DIRECTION ( 'NONE',  ( -1.000000000000000000, -0.000000000000000000, -0.000000000000000000 ) ) ;
#2792 = CARTESIAN_POINT ( 'NONE',  ( -4.743843029824828861, 13.17239914596749450, 14.42453085894499232 ) ) ;
#2793 = CARTESIAN_POINT ( 'NONE',  ( -8.877401133907129704, 4.579542530753038854, 16.85113791807854611 ) ) ;
#2795 = CIRCLE ( 'NONE', #3809, 17.72919999999999874 ) ;
#2794 = CARTESIAN_POINT ( 'NONE',  ( -8.464561979789474222, -4.312909747525728754, 17.39999999999997016 ) ) ;
#2796 = CARTESIAN_POINT ( 'NONE',  ( -164.8603691185176388, 2.150052187497858647, 14.84510948406350472 ) ) ;
#2797 = CARTESIAN_POINT ( 'NONE',  ( -13.82664651025767100, 8.841785722321537477, 33.78975485534073897 ) ) ;
#2798 = CARTESIAN_POINT ( 'NONE',  ( 14.26974319298268767, -1.607813917172876916, 38.35714285714287541 ) ) ;
#2799 = CARTESIAN_POINT ( 'NONE',  ( 4.623906867372411078, -13.21436662431711717, 33.42857142857143060 ) ) ;
#2800 = ORIENTED_EDGE ( 'NONE', *, *, #4948, .F. ) ;
#2801 = EDGE_CURVE ( 'NONE', #3385, #4723, #596, .T. ) ;
#2802 = AXIS2_PLACEMENT_3D ( 'NONE', #5191, #5142, #5952 ) ;
#2803 = CARTESIAN_POINT ( 'NONE',  ( 16.30827793483735633, -1.837501619626142890, 44.35714285714287541 ) ) ;
#2804 = DIRECTION ( 'NONE',  ( 0.000000000000000000, 0.000000000000000000, 1.000000000000000000 ) ) ;
#2805 = CIRCLE ( 'NONE', #8595, 18.00000000000000000 ) ;
#2806 = CARTESIAN_POINT ( 'NONE',  ( 13.89598863503046111, -8.731428362939032795, 32.78571428571430602 ) ) ;
#2807 = DIRECTION ( 'NONE',  ( 1.000000000000000000, 4.755747939841215952E-17, -0.000000000000000000 ) ) ;
#2808 =( NAMED_UNIT ( * ) SI_UNIT ( $, .STERADIAN. ) SOLID_ANGLE_UNIT ( ) );
#2809 = FACE_OUTER_BOUND ( 'NONE', #4327, .T. ) ;
#2810 = CARTESIAN_POINT ( 'NONE',  ( 7.063212654743467489, 7.063212654743557195, 0.7499999999999762412 ) ) ;
#2811 = CARTESIAN_POINT ( 'NONE',  ( 6.751237864895159646, -6.683790977649239906, 11.49886208192146775 ) ) ;
#2812 = EDGE_CURVE ( 'NONE', #6711, #7540, #2172, .T. ) ;
#2813 = CARTESIAN_POINT ( 'NONE',  ( 9.837026868206066865, -5.012215536711391195, 10.35000000000002274 ) ) ;
#2814 = CARTESIAN_POINT ( 'NONE',  ( 5.543385399275644332, 15.44746603149420494, 11.07546914105500768 ) ) ;
#2815 = CARTESIAN_POINT ( 'NONE',  ( 5.420364854932001819, 15.49051278174644430, 31.07142857142857295 ) ) ;
#2816 = CIRCLE ( 'NONE', #4642, 18.00000000000000355 ) ;
#2817 = VECTOR ( 'NONE', #1506, 1000.000000000000000 ) ;
#2818 = CARTESIAN_POINT ( 'NONE',  ( -13.82664651025767100, 8.841785722321537477, 3.789754855340718542 ) ) ;
#2819 = CARTESIAN_POINT ( 'NONE',  ( 1.607813917173038121, -14.26974319298267346, 27.64285714285714590 ) ) ;
#2820 = CARTESIAN_POINT ( 'NONE',  ( 5.284464991282756152, -15.10213328493384743, 9.428571428571425272 ) ) ;
#2821 = CARTESIAN_POINT ( 'NONE',  ( 8.512513224245308763, 13.54758718765259040, 43.28571428571429180 ) ) ;
#2822 = ORIENTED_EDGE ( 'NONE', *, *, #5504, .F. ) ;
#2823 = CARTESIAN_POINT ( 'NONE',  ( 4.766900247265192903, 9.355568503977902850, 15.60000000000000320 ) ) ;
#2824 = ORIENTED_EDGE ( 'NONE', *, *, #4691, .T. ) ;
#2825 = CARTESIAN_POINT ( 'NONE',  ( 13.54758718765249803, 8.512513224245457977, 25.71428571428571885 ) ) ;
#2826 = CARTESIAN_POINT ( 'NONE',  ( -7.750357176954294935, 12.08964793087877787, 2.210245144659280569 ) ) ;
#2827 = CARTESIAN_POINT ( 'NONE',  ( -9.333916720356675967, -4.809394265263095214, 3.398862081921444123 ) ) ;
#2828 = APPLICATION_PROTOCOL_DEFINITION ( 'draft international standard', 'automotive_design', 1998, #2233 ) ;
#2829 = PRODUCT_RELATED_PRODUCT_CATEGORY ( 'part', '', ( #2773 ) ) ;
#2830 = CARTESIAN_POINT ( 'NONE',  ( -13.21436662431716869, 4.623906867372262752, 23.57142857142857650 ) ) ;
#2831 = AXIS2_PLACEMENT_3D ( 'NONE', #2976, #9242, #6952 ) ;
#2832 = CARTESIAN_POINT ( 'NONE',  ( 10.06191849875406064, 10.24623928997363187, 21.49595943037356705 ) ) ;
#2833 = VERTEX_POINT ( 'NONE', #3947 ) ;
#2834 =( NAMED_UNIT ( * ) PLANE_ANGLE_UNIT ( ) SI_UNIT ( $, .RADIAN. ) );
#2835 = CARTESIAN_POINT ( 'NONE',  ( 4.853079829769881393, 13.20943203255562359, 48.72999999999996845 ) ) ;
#2836 = CARTESIAN_POINT ( 'NONE',  ( 9.859792900771104485, -4.967534682030585458, 17.34886208192141765 ) ) ;
#2837 = CARTESIAN_POINT ( 'NONE',  ( 1.607813917173038121, -14.26974319298267346, 3.642857142857144126 ) ) ;
#2838 = CARTESIAN_POINT ( 'NONE',  ( 7.424621202458790314, -7.424621202458697944, 7.500000000000007105 ) ) ;
#2839 = CARTESIAN_POINT ( 'NONE',  ( 7.390897758835871301, -7.458344646081624063, 12.50113791807859265 ) ) ;
#2840 = DIRECTION ( 'NONE',  ( 0.000000000000000000, 1.000000000000000000, 0.000000000000000000 ) ) ;
#2841 = VERTEX_POINT ( 'NONE', #797 ) ;
#2842 = AXIS2_PLACEMENT_3D ( 'NONE', #3609, #6028, #9208 ) ;
#2843 = CARTESIAN_POINT ( 'NONE',  ( -1.642561882922479732, 10.37072757624896191, 9.299999999999975842 ) ) ;
#2844 = CARTESIAN_POINT ( 'NONE',  ( -8.404922754268618235, -13.61519076058357491, 36.28167371608785174 ) ) ;
#2845 = CARTESIAN_POINT ( 'NONE',  ( -3.603708530703266799, 13.57059942033907873, 48.73000000000004661 ) ) ;
#2846 = CARTESIAN_POINT ( 'NONE',  ( -163.5589117782047595, -0.8318236505920658663, 12.97488054948080993 ) ) ;
#2847 = ADVANCED_FACE ( 'NONE', ( #6990 ), #1475, .T. ) ;
#2848 = CARTESIAN_POINT ( 'NONE',  ( -4.619798703721853528, -13.59724543428036725, 18.06738800180213644 ) ) ;
#2849 = CARTESIAN_POINT ( 'NONE',  ( 9.873755945037075321, 1.513077731353043243, 15.05113791807855961 ) ) ;
#2850 = CARTESIAN_POINT ( 'NONE',  ( 7.063212654743467489, 7.063212654743557195, 12.75000000000000533 ) ) ;
#2851 = FACE_OUTER_BOUND ( 'NONE', #8992, .T. ) ;
#2852 = CARTESIAN_POINT ( 'NONE',  ( -9.899494936611716867, 9.899494936611610285, 42.00000000000000000 ) ) ;
#2853 = CARTESIAN_POINT ( 'NONE',  ( 14.26974319298268767, -1.607813917172876916, 38.35714285714287541 ) ) ;
#2854 = EDGE_LOOP ( 'NONE', ( #4126, #5157 ) ) ;
#2855 = CARTESIAN_POINT ( 'NONE',  ( 11.31370849898482334, -11.31370849898469366, 39.00000000000000000 ) ) ;
#2856 = CYLINDRICAL_SURFACE ( 'NONE', #841, 0.9906000000000003691 ) ;
#2857 = CARTESIAN_POINT ( 'NONE',  ( -5.420364854931999155, -15.49051278174644253, 28.07142857142857295 ) ) ;
#2858 = FACE_OUTER_BOUND ( 'NONE', #6255, .T. ) ;
#2859 =( NAMED_UNIT ( * ) PLANE_ANGLE_UNIT ( ) SI_UNIT ( $, .RADIAN. ) );
#2860 = PLANE ( 'NONE',  #9099 ) ;
#2861 = CARTESIAN_POINT ( 'NONE',  ( 1.562606840307832368, 9.865911304835503159, 6.449999999999969091 ) ) ;
#2862 = CARTESIAN_POINT ( 'NONE',  ( -7.027753727702738651, -7.098671581784262941, 12.24886208192144998 ) ) ;
#2863 = CARTESIAN_POINT ( 'NONE',  ( 1.727091770866550968, 10.90442828429187294, 15.44999999999997797 ) ) ;
#2864 = CARTESIAN_POINT ( 'NONE',  ( -15.53355953199861794, -5.297344310588530725, 20.93261199819787066 ) ) ;
#2865 = CARTESIAN_POINT ( 'NONE',  ( 15.49051278174638036, 5.420364854932175014, 37.92857142857143060 ) ) ;
#2866 = VECTOR ( 'NONE', #6199, 1000.000000000000000 ) ;
#2867 = CARTESIAN_POINT ( 'NONE',  ( 5.543385399275644332, 15.44746603149420494, 23.07546914105501301 ) ) ;
#2868 = CARTESIAN_POINT ( 'NONE',  ( -1.567502665446231180, -13.91197093850540334, 21.85714285714286120 ) ) ;
#2869 = ADVANCED_FACE ( 'NONE', ( #2395 ), #704, .T. ) ;
#2870 = CARTESIAN_POINT ( 'NONE',  ( -8.731428362939189114, 13.89598863503036341, 0.2142857142857168273 ) ) ;
#2871 = CARTESIAN_POINT ( 'NONE',  ( 55.99999999999996447, 0.000000000000000000, 8.000000000000000000 ) ) ;
#2872 = ORIENTED_EDGE ( 'NONE', *, *, #2433, .T. ) ;
#2873 = CARTESIAN_POINT ( 'NONE',  ( 1.642561882922480621, -10.37072757624892638, 16.80000000000003624 ) ) ;
#2874 = EDGE_LOOP ( 'NONE', ( #5790, #7225 ) ) ;
#2875 = DIRECTION ( 'NONE',  ( -6.162975822039154730E-33, -0.4999999999999991118, 0.8660254037844391517 ) ) ;
#2876 = EDGE_CURVE ( 'NONE', #1178, #9145, #10152, .T. ) ;
#2877 = CARTESIAN_POINT ( 'NONE',  ( 9.938986324564400121, 12.66818340422679157, 51.38745637415366474 ) ) ;
#2878 = CARTESIAN_POINT ( 'NONE',  ( -5.012215536711506658, 9.837026868206027785, 15.14999999999998259 ) ) ;
#2879 = CARTESIAN_POINT ( 'NONE',  ( 11.60466159355862104, 11.60466159355875071, 1.500000000000003553 ) ) ;
#2880 = CARTESIAN_POINT ( 'NONE',  ( -4.623906867372410190, 13.21436662431711895, 24.42857142857143060 ) ) ;
#2881 = CARTESIAN_POINT ( 'NONE',  ( 1.441234910513245149, 13.92619789766829008, 44.85310228751641404 ) ) ;
#2882 = ORIENTED_EDGE ( 'NONE', *, *, #5772, .F. ) ;
#2883 = CARTESIAN_POINT ( 'NONE',  ( -43.00000000000002842, 1.501835218140771832E-15, -13.00000000000000178 ) ) ;
#2884 = CARTESIAN_POINT ( 'NONE',  ( -16.32287076676382398, 1.707986654103809343, 7.353102287516419366 ) ) ;
#2885 = ADVANCED_FACE ( 'NONE', ( #7092 ), #7730, .F. ) ;
#2886 = FACE_OUTER_BOUND ( 'NONE', #8049, .T. ) ;
#2887 = CARTESIAN_POINT ( 'NONE',  ( 4.724406229267374968, 9.377220287599064008, 16.59886208192139989 ) ) ;
#2888 = CARTESIAN_POINT ( 'NONE',  ( 1.727091770866550968, 10.90442828429187294, 9.449999999999988631 ) ) ;
#2889 = CARTESIAN_POINT ( 'NONE',  ( -1.595456901104623348, 10.37818827243066622, 11.30113791807855961 ) ) ;
#2890 = DIRECTION ( 'NONE',  ( 0.000000000000000000, -8.191099868251446680E-34, -1.000000000000000000 ) ) ;
#2891 = CARTESIAN_POINT ( 'NONE',  ( -14.25515036105622890, 1.737328882695209575, 33.36118342676929416 ) ) ;
#2892 = ORIENTED_EDGE ( 'NONE', *, *, #8368, .T. ) ;
#2893 = CARTESIAN_POINT ( 'NONE',  ( 9.859792900771104485, -4.967534682030589011, 2.348862081921457623 ) ) ;
#2894 = CARTESIAN_POINT ( 'NONE',  ( -15.14410076328353227, 5.164528828830164287, 49.56738800180214355 ) ) ;
#2895 = CARTESIAN_POINT ( 'NONE',  ( -3.886497728173464061, 15.50039264458562904, 48.73000000000005372 ) ) ;
#2896 = PLANE ( 'NONE',  #885 ) ;
#2897 = CARTESIAN_POINT ( 'NONE',  ( 13.25633410266679313, -4.503970704919842305, 22.56738800180214000 ) ) ;
#2898 = CARTESIAN_POINT ( 'NONE',  ( -9.873755945037078874, -1.513077731353019706, 10.55113791807857204 ) ) ;
#2899 = CARTESIAN_POINT ( 'NONE',  ( 1.439022436064387511, -9.390499931835512015, 0.8011379180785925813 ) ) ;
#2900 = CARTESIAN_POINT ( 'NONE',  ( -166.3099971560734218, -1.710604296556395898, 12.88720430579052767 ) ) ;
#2901 = CARTESIAN_POINT ( 'NONE',  ( 15.91362231745475597, 1.665163862720026255, 42.14689771248358596 ) ) ;
#2902 = CARTESIAN_POINT ( 'NONE',  ( 13.55419868402807992, 4.742819248065648807, 37.92857142857143060 ) ) ;
#2903 = EDGE_CURVE ( 'NONE', #10190, #9396, #6449, .T. ) ;
#2904 = CARTESIAN_POINT ( 'NONE',  ( -1.693770420379220099, -13.89774397934251837, 1.861183426769295490 ) ) ;
#2905 = VERTEX_POINT ( 'NONE', #9384 ) ;
#2906 = CARTESIAN_POINT ( 'NONE',  ( 15.14410076328353227, -5.164528828830166063, 4.567388001802134667 ) ) ;
#2907 = CARTESIAN_POINT ( 'NONE',  ( -3.334129424850329482, 15.49830167892402066, 1.394172777290140936E-15 ) ) ;
#2908 = CARTESIAN_POINT ( 'NONE',  ( -16.30827793483735988, 1.837501619626141780, 23.35714285714286476 ) ) ;
#2909 = LINE ( 'NONE', #3744, #9941 ) ;
#2910 = CARTESIAN_POINT ( 'NONE',  ( 9.355568503977840678, 4.766900247265305701, 0.9000000000000119016 ) ) ;
#2911 = CARTESIAN_POINT ( 'NONE',  ( 9.865911304835474738, 1.562606840307948719, 4.049999999999988276 ) ) ;
#2912 = CARTESIAN_POINT ( 'NONE',  ( 4.270415729527831772, 8.486213763410694000, 19.59886208192144963 ) ) ;
#2913 = CARTESIAN_POINT ( 'NONE',  ( 10.37072757624895836, -1.642561882922356498, 13.19999999999998863 ) ) ;
#2914 = CARTESIAN_POINT ( 'NONE',  ( -16.29368510291090288, 1.967016585148476215, 21.36118342676929771 ) ) ;
#2915 = CARTESIAN_POINT ( 'NONE',  ( -13.89598863503046111, 8.731428362939027465, 47.78571428571430602 ) ) ;
#2916 = CARTESIAN_POINT ( 'NONE',  ( -61.27000000000002444, -1.260068276681486816E-14, -4.781924897640271809E-16 ) ) ;
#2917 = CARTESIAN_POINT ( 'NONE',  ( -13.61519076058348254, -8.404922754268771001, 26.71832628391215536 ) ) ;
#2918 = CARTESIAN_POINT ( 'NONE',  ( 13.55419868402807992, 4.742819248065648807, 25.92857142857142705 ) ) ;
#2919 = CARTESIAN_POINT ( 'NONE',  ( -11.60466159355861926, -11.60466159355875249, 4.500000000000005329 ) ) ;
#2920 = CARTESIAN_POINT ( 'NONE',  ( -15.49051278174638036, -5.420364854932175902, 40.92857142857145192 ) ) ;
#2921 = ORIENTED_EDGE ( 'NONE', *, *, #8517, .T. ) ;
#2922 = EDGE_CURVE ( 'NONE', #3401, #5632, #5460, .T. ) ;
#2923 = CARTESIAN_POINT ( 'NONE',  ( -9.837026868206066865, 5.012215536711413399, 14.84999999999999787 ) ) ;
#2924 = CARTESIAN_POINT ( 'NONE',  ( -4.995402070941133310, -13.58603705635637304, 0.000000000000000000 ) ) ;
#2925 = PLANE ( 'NONE',  #2986 ) ;
#2926 = COLOUR_RGB ( '', 0.31764706, 0.68627451, 0.89019608) ;
#2927 = CARTESIAN_POINT ( 'NONE',  ( -13.47998361472151174, -8.620103694222146729, 48.71024514465926814 ) ) ;
#2928 = CARTESIAN_POINT ( 'NONE',  ( 10.37072757624895836, -1.642561882922356498, 16.19999999999999218 ) ) ;
#2929 = CARTESIAN_POINT ( 'NONE',  ( 1.791431617652837316, 15.89939535829188877, 0.8571428571428549859 ) ) ;
#2930 = CARTESIAN_POINT ( 'NONE',  ( -11.22385875690717327, 11.40355824106234550, 46.00404056962644006 ) ) ;
#2931 = SHAPE_DEFINITION_REPRESENTATION ( #393, #3956 ) ;
#2932 = CARTESIAN_POINT ( 'NONE',  ( 1.567502665446232957, 13.91197093850540156, 18.85714285714285765 ) ) ;
#2933 = CARTESIAN_POINT ( 'NONE',  ( 9.809645194534072132, -9.989344678689256796, 25.00404056962644006 ) ) ;
#2934 = CARTESIAN_POINT ( 'NONE',  ( 10.06191849875406064, 10.24623928997363187, 45.49595943037356705 ) ) ;
#2935 = VERTEX_POINT ( 'NONE', #10104 ) ;
#2936 = FACE_OUTER_BOUND ( 'NONE', #6556, .T. ) ;
#2937 = CARTESIAN_POINT ( 'NONE',  ( 1.967016585148662289, -16.29368510291087091, 29.63881657323071295 ) ) ;
#2938 = DIRECTION ( 'NONE',  ( -1.000000000000000000, 0.000000000000000000, 0.000000000000000000 ) ) ;
#2939 = CARTESIAN_POINT ( 'NONE',  ( -7.458344646081709328, 7.390897758835805575, 15.99886208192142512 ) ) ;
#2940 = CARTESIAN_POINT ( 'NONE',  ( -7.340858601237953529, -11.92174236212700222, 48.28167371608785174 ) ) ;
#2941 = CARTESIAN_POINT ( 'NONE',  ( 10.90442828429183919, 1.727091770866679532, 1.049999999999966738 ) ) ;
#2942 = CARTESIAN_POINT ( 'NONE',  ( 10.91227292449344155, 1.677562661911773167, 18.05113791807859513 ) ) ;
#2943 = DIRECTION ( 'NONE',  ( 1.000000000000000000, 0.000000000000000000, 0.000000000000000000 ) ) ;
#2944 = CARTESIAN_POINT ( 'NONE',  ( -1.478298951650703019, 14.28433602490913579, 28.64689771248357886 ) ) ;
#2945 = CARTESIAN_POINT ( 'NONE',  ( -156.0000000000000284, -2.164934898019055569E-14, 0.000000000000000000 ) ) ;
#2946 = ORIENTED_EDGE ( 'NONE', *, *, #8692, .F. ) ;
#2947 = CARTESIAN_POINT ( 'NONE',  ( -15.88516839912898071, -1.917699372586004980, 49.13881657323070584 ) ) ;
#2948 = CARTESIAN_POINT ( 'NONE',  ( 7.424621202458790314, -7.424621202458697944, 1.500000000000001332 ) ) ;
#2949 = CARTESIAN_POINT ( 'NONE',  ( -166.6500000000000341, -1.532656777835077474E-15, 13.00000000000000355 ) ) ;
#2950 = CARTESIAN_POINT ( 'NONE',  ( -7.340858601237953529, -11.92174236212700222, 12.28167371608784997 ) ) ;
#2951 = CARTESIAN_POINT ( 'NONE',  ( 10.91227292449344155, 1.677562661911773390, 0.05113791807855379290 ) ) ;
#2952 = CARTESIAN_POINT ( 'NONE',  ( -4.355403765523468529, -8.442910196168346815, 7.101137918078564759 ) ) ;
#2953 = CARTESIAN_POINT ( 'NONE',  ( -108.0000000000000426, 15.99999999999999289, 1.959434878635764737E-15 ) ) ;
#2954 = CARTESIAN_POINT ( 'NONE',  ( -8.620103694221995738, -13.47998361472161299, 44.28975485534073186 ) ) ;
#2955 = CARTESIAN_POINT ( 'NONE',  ( -7.448449071214644945, -11.85413878919601771, 40.28571428571428470 ) ) ;
#2956 = CARTESIAN_POINT ( 'NONE',  ( 7.529642458189280241, -12.22833218042435099, 1.218326283912148922 ) ) ;
#2957 = ORIENTED_EDGE ( 'NONE', *, *, #4838, .T. ) ;
#2958 = CARTESIAN_POINT ( 'NONE',  ( 1.665163862719847732, 15.91362231745477374, 8.853102287516419366 ) ) ;
#2959 = DIRECTION ( 'NONE',  ( 1.000000000000000000, 4.755747939841215952E-17, -0.000000000000000000 ) ) ;
#2960 = CARTESIAN_POINT ( 'NONE',  ( 5.284464991282756152, -15.10213328493384743, 33.42857142857143060 ) ) ;
#2961 = DIRECTION ( 'NONE',  ( 0.000000000000000000, 0.000000000000000000, -1.000000000000000000 ) ) ;
#2962 = COLOUR_RGB ( '', 0.31764706, 0.68627451, 0.89019608) ;
#2963 = CARTESIAN_POINT ( 'NONE',  ( 5.012215536711511987, -9.837026868205999364, 1.650000000000006128 ) ) ;
#2964 = CARTESIAN_POINT ( 'NONE',  ( -8.464561979789474222, -4.312909747525728754, 11.39999999999996660 ) ) ;
#2965 = CARTESIAN_POINT ( 'NONE',  ( -4.579542530753125895, 8.877401133907090625, 16.14886208192145389 ) ) ;
#2966 = CARTESIAN_POINT ( 'NONE',  ( -16.00000000000000000, 0.000000000000000000, 68.00000000000000000 ) ) ;
#2967 = CARTESIAN_POINT ( 'NONE',  ( -16.30827793483735988, 1.837501619626141780, 47.35714285714286120 ) ) ;
#2968 = CARTESIAN_POINT ( 'NONE',  ( -8.621071003556675549, 13.96533075980314642, 22.21832628391215181 ) ) ;
#2969 = AXIS2_PLACEMENT_3D ( 'NONE', #6925, #6153, #746 ) ;
#2970 = VERTEX_POINT ( 'NONE', #6107 ) ;
#2971 = CARTESIAN_POINT ( 'NONE',  ( -8.731428362939189114, 13.89598863503036341, 12.21428571428571885 ) ) ;
#2972 = FACE_OUTER_BOUND ( 'NONE', #6686, .T. ) ;
#2973 = ORIENTED_EDGE ( 'NONE', *, *, #8348, .T. ) ;
#2974 = EDGE_CURVE ( 'NONE', #9051, #8798, #8703, .T. ) ;
#2975 = CARTESIAN_POINT ( 'NONE',  ( 7.424621202458790314, -7.424621202458697944, 19.50000000000001776 ) ) ;
#2976 = CARTESIAN_POINT ( 'NONE',  ( 0.000000000000000000, 0.000000000000000000, 0.000000000000000000 ) ) ;
#2977 = CARTESIAN_POINT ( 'NONE',  ( -11.60466159355861748, -11.60466159355874893, 40.50000000000000000 ) ) ;
#2978 = AXIS2_PLACEMENT_3D ( 'NONE', #5287, #8445, #2804 ) ;
#2979 = SURFACE_SIDE_STYLE ('',( #3763 ) ) ;
#2980 =( GEOMETRIC_REPRESENTATION_CONTEXT ( 3 ) GLOBAL_UNCERTAINTY_ASSIGNED_CONTEXT ( ( #1844 ) ) GLOBAL_UNIT_ASSIGNED_CONTEXT ( ( #1839, #5753, #6718 ) ) REPRESENTATION_CONTEXT ( 'NONE', 'WORKASPACE' ) );
#2981 = AXIS2_PLACEMENT_3D ( 'NONE', #7760, #6860, #10083 ) ;
#2982 = CARTESIAN_POINT ( 'NONE',  ( 10.37818827243067510, -1.595456901104499448, 11.19886208192145816 ) ) ;
#2983 = CARTESIAN_POINT ( 'NONE',  ( -8.731428362939189114, 13.89598863503036341, 0.2142857142857168273 ) ) ;
#2984 = CARTESIAN_POINT ( 'NONE',  ( -15.53355953199861794, -5.297344310588530725, 44.93261199819787777 ) ) ;
#2985 = CARTESIAN_POINT ( 'NONE',  ( -13.55419868402807992, -4.742819248065651472, 22.92857142857143060 ) ) ;
#2986 = AXIS2_PLACEMENT_3D ( 'NONE', #5250, #4487, #7641 ) ;
#2987 = CARTESIAN_POINT ( 'NONE',  ( 8.464561979789474222, 4.312909747525755400, 6.899999999999961275 ) ) ;
#2988 = AXIS2_PLACEMENT_3D ( 'NONE', #4365, #5955, #6053 ) ;
#2989 = PRESENTATION_LAYER_ASSIGNMENT (  '', '', ( #7446 ) ) ;
#2990 = CARTESIAN_POINT ( 'NONE',  ( 13.89774397934249706, 1.693770420379375308, 46.13881657323070584 ) ) ;
#2991 = ORIENTED_EDGE ( 'NONE', *, *, #457, .F. ) ;
#2992 = CARTESIAN_POINT ( 'NONE',  ( -165.0000000000000284, -6.071532165918824830E-15, 0.000000000000000000 ) ) ;
#2993 = CARTESIAN_POINT ( 'NONE',  ( 5.404401153735178376, -15.06016580658422477, 23.42453085894499409 ) ) ;
#2994 = CARTESIAN_POINT ( 'NONE',  ( 8.731428362939189114, -13.89598863503035986, 3.214285714285716633 ) ) ;
#2995 = CARTESIAN_POINT ( 'NONE',  ( -9.390499931835536884, 1.439022436064298249, 12.69886208192145816 ) ) ;
#2996 = CARTESIAN_POINT ( 'NONE',  ( 16.32287076676382043, -1.707986654103810897, 28.35310228751642825 ) ) ;
#2997 = CARTESIAN_POINT ( 'NONE',  ( 7.424621202458790314, -7.424621202458697944, 1.500000000000001332 ) ) ;
#2998 = CARTESIAN_POINT ( 'NONE',  ( 1.595456901104624459, -10.37818827243064490, 15.80113791807855961 ) ) ;
#2999 = CARTESIAN_POINT ( 'NONE',  ( -5.986002070941136566, -13.58603705635637482, -1.270000000000007123 ) ) ;
#3000 = CARTESIAN_POINT ( 'NONE',  ( -1.478298951650703019, 14.28433602490913579, 34.64689771248358596 ) ) ;
#3001 = CARTESIAN_POINT ( 'NONE',  ( -8.404922754268618235, -13.61519076058357491, 48.28167371608785174 ) ) ;
#3002 = ADVANCED_FACE ( 'NONE', ( #8499 ), #10202, .T. ) ;
#3003 = CARTESIAN_POINT ( 'NONE',  ( -4.766900247265192014, -9.355568503977876205, 2.099999999999990763 ) ) ;
#3004 = CARTESIAN_POINT ( 'NONE',  ( 1.791431617652837316, 15.89939535829188877, 30.85714285714286120 ) ) ;
#3005 = AXIS2_PLACEMENT_3D ( 'NONE', #2372, #1708, #883 ) ;
#3006 = DIRECTION ( 'NONE',  ( 0.000000000000000000, -6.338944243255235518E-49, 1.000000000000000000 ) ) ;
#3007 = CARTESIAN_POINT ( 'NONE',  ( -4.355403765523468529, -8.442910196168346815, 16.10113791807856742 ) ) ;
#3008 = CARTESIAN_POINT ( 'NONE',  ( -9.873755945037078874, -1.513077731353019706, 4.551137918078585365 ) ) ;
#3009 = CARTESIAN_POINT ( 'NONE',  ( -164.7162546839571462, -2.135798021625797460, 12.82338259142922432 ) ) ;
#3010 = CARTESIAN_POINT ( 'NONE',  ( -9.899494936611716867, 9.899494936611610285, 48.00000000000000000 ) ) ;
#3011 = CARTESIAN_POINT ( 'NONE',  ( -7.529642458189277576, 12.22833218042435455, -1.781673716087850634 ) ) ;
#3012 = ORIENTED_EDGE ( 'NONE', *, *, #9611, .F. ) ;
#3013 = CARTESIAN_POINT ( 'NONE',  ( 15.88516839912898071, 1.917699372586004092, 4.138816573230708507 ) ) ;
#3014 = CARTESIAN_POINT ( 'NONE',  ( 55.99999999999996447, 9.797174393178825657E-16, -8.000000000000000000 ) ) ;
#3015 = CARTESIAN_POINT ( 'NONE',  ( -11.60466159355861926, -11.60466159355875249, 28.50000000000001066 ) ) ;
#3016 = DIRECTION ( 'NONE',  ( -1.000000000000000000, 0.000000000000000000, 0.000000000000000000 ) ) ;
#3017 = DIRECTION ( 'NONE',  ( -1.000000000000000000, 0.000000000000000000, 0.000000000000000000 ) ) ;
#3018 = CIRCLE ( 'NONE', #6628, 13.00000000000000000 ) ;
#3019 = PRODUCT_RELATED_PRODUCT_CATEGORY ( 'part', '', ( #3433 ) ) ;
#3020 = CARTESIAN_POINT ( 'NONE',  ( -15.44569104238500046, -1.018491042384999545, -1.270000000000007123 ) ) ;
#3021 = CARTESIAN_POINT ( 'NONE',  ( -9.383039235653820143, 1.486127417882155521, 5.700000000000038369 ) ) ;
#3022 = CARTESIAN_POINT ( 'NONE',  ( 9.858066664633883036, 1.612135949262857526, 17.04886208192142760 ) ) ;
#3023 = CARTESIAN_POINT ( 'NONE',  ( -58.00000000000002132, 7.703719777548943412E-30, -1.059261469412979719E-30 ) ) ;
#3024 = CARTESIAN_POINT ( 'NONE',  ( 16.29368510291089223, -1.967016585148476882, 18.36118342676929771 ) ) ;
#3025 = CARTESIAN_POINT ( 'NONE',  ( -15.49051278174638036, -5.420364854932175902, 46.92857142857142350 ) ) ;
#3026 = SURFACE_STYLE_USAGE ( .BOTH. , #3753 ) ;
#3027 = CARTESIAN_POINT ( 'NONE',  ( -15.91362231745475597, -1.665163862720028254, 21.14689771248358241 ) ) ;
#3028 = CARTESIAN_POINT ( 'NONE',  ( -15.49051278174638036, -5.420364854932175902, 22.92857142857142705 ) ) ;
#3029 = CARTESIAN_POINT ( 'NONE',  ( -68.00000000000001421, 2.204364238465235822E-15, -18.00000000000000355 ) ) ;
#3030 = CARTESIAN_POINT ( 'NONE',  ( 5.012215536711511987, -9.837026868205999364, 13.65000000000003233 ) ) ;
#3031 = VERTEX_POINT ( 'NONE', #3172 ) ;
#3032 = CARTESIAN_POINT ( 'NONE',  ( -170.0000000000000284, -8.084771497730068080E-15, 0.000000000000000000 ) ) ;
#3033 = AXIS2_PLACEMENT_3D ( 'NONE', #7911, #5431, #4566 ) ;
#3034 = CARTESIAN_POINT ( 'NONE',  ( -5.056896391392315948, 9.814260835640991942, 13.14886208192146633 ) ) ;
#3035 = CARTESIAN_POINT ( 'NONE',  ( 16.30827793483735633, -1.837501619626142890, 2.357142857142856762 ) ) ;
#3036 = CARTESIAN_POINT ( 'NONE',  ( -11.69682198916834892, -11.51250119794901394, 44.50404056962644006 ) ) ;
#3037 = APPLICATION_PROTOCOL_DEFINITION ( 'draft international standard', 'automotive_design', 1998, #257 ) ;
#3038 = CARTESIAN_POINT ( 'NONE',  ( -9.899494936611716867, 9.899494936611610285, 30.00000000000000355 ) ) ;
#3039 = CARTESIAN_POINT ( 'NONE',  ( -7.556039541191334585, -11.78653521626503320, 38.28975485534072476 ) ) ;
#3040 = CARTESIAN_POINT ( 'NONE',  ( -8.900167166472160218, 4.534861676072235781, 11.84999999999997478 ) ) ;
#3041 = CARTESIAN_POINT ( 'NONE',  ( -10.06191849875405531, -10.24623928997363542, 42.49595943037355994 ) ) ;
#3042 = VERTEX_POINT ( 'NONE', #5497 ) ;
#3043 = CARTESIAN_POINT ( 'NONE',  ( -9.899494936611716867, 9.899494936611610285, 0.000000000000000000 ) ) ;
#3044 = CARTESIAN_POINT ( 'NONE',  ( -15.88516839912898071, -1.917699372586004980, 19.13881657323070584 ) ) ;
#3045 = CARTESIAN_POINT ( 'NONE',  ( 15.49051278174637858, 5.420364854932174126, 7.928571428571430602 ) ) ;
#3046 = CARTESIAN_POINT ( 'NONE',  ( -6.751237864895158758, 6.683790977649255005, 12.99886208192142512 ) ) ;
#3047 = CARTESIAN_POINT ( 'NONE',  ( -5.297344310588352201, -15.53355953199867301, 24.06738800180213644 ) ) ;
#3048 = CARTESIAN_POINT ( 'NONE',  ( 1.727091770866550968, 10.90442828429187294, 0.4499999999999856337 ) ) ;
#3049 = CARTESIAN_POINT ( 'NONE',  ( 4.809394265263009061, 9.333916720356739916, 14.60113791807856920 ) ) ;
#3050 = PLANE ( 'NONE',  #2981 ) ;
#3051 = CARTESIAN_POINT ( 'NONE',  ( -7.529642458189277576, 12.22833218042435455, 46.21832628391216247 ) ) ;
#3052 = CARTESIAN_POINT ( 'NONE',  ( -7.750357176954294935, 12.08964793087877787, 8.210245144659282346 ) ) ;
#3053 = CARTESIAN_POINT ( 'NONE',  ( -5.012215536711508435, 9.837026868206027785, 3.149999999999958611 ) ) ;
#3054 = CARTESIAN_POINT ( 'NONE',  ( 5.420364854932001819, 15.49051278174644430, 31.07142857142857295 ) ) ;
#3055 = CARTESIAN_POINT ( 'NONE',  ( -58.00000000000002842, 7.703719777548943412E-30, -1.059261469412979719E-30 ) ) ;
#3056 = CARTESIAN_POINT ( 'NONE',  ( 4.619798703721856192, 13.59724543428036725, 27.06738800180213644 ) ) ;
#3057 = CARTESIAN_POINT ( 'NONE',  ( 10.91227292449344155, 1.677562661911774944, 9.051137918078573819 ) ) ;
#3058 = CARTESIAN_POINT ( 'NONE',  ( -4.355403765523468529, -8.442910196168352144, 4.101137918078561206 ) ) ;
#3059 = FACE_BOUND ( 'NONE', #8461, .T. ) ;
#3060 = CARTESIAN_POINT ( 'NONE',  ( 1.707986654103998303, -16.32287076676380266, 43.64689771248358596 ) ) ;
#3061 = CARTESIAN_POINT ( 'NONE',  ( -7.529642458189277576, 12.22833218042435455, 10.21832628391215358 ) ) ;
#3062 = CARTESIAN_POINT ( 'NONE',  ( 1.567502665446232957, 13.91197093850540156, 48.85714285714286120 ) ) ;
#3063 = VERTEX_POINT ( 'NONE', #9285 ) ;
#3064 = CARTESIAN_POINT ( 'NONE',  ( 1.665163862719847732, 15.91362231745477374, 14.85310228751642470 ) ) ;
#3065 = CARTESIAN_POINT ( 'NONE',  ( -31.74999999999994316, 2.866884953888006423E-33, 3.500000000000000000 ) ) ;
#3066 = EDGE_CURVE ( 'NONE', #6680, #9282, #1927, .T. ) ;
#3067 = CARTESIAN_POINT ( 'NONE',  ( 1.837501619626330074, -16.30827793483733501, 45.64285714285716011 ) ) ;
#3068 = DIRECTION ( 'NONE',  ( 0.000000000000000000, -8.191099868251446680E-34, -1.000000000000000000 ) ) ;
#3069 = DIRECTION ( 'NONE',  ( 1.000000000000000000, -1.842239752758738928E-31, -1.840628461782073167E-32 ) ) ;
#3070 = CARTESIAN_POINT ( 'NONE',  ( 8.877401133907127928, -4.579542530753017537, 0.3511379180785880183 ) ) ;
#3071 = CARTESIAN_POINT ( 'NONE',  ( 7.027753727702739539, 7.098671581784283369, 13.74886208192144643 ) ) ;
#3072 = CARTESIAN_POINT ( 'NONE',  ( -68.00000000000001421, 0.000000000000000000, 0.000000000000000000 ) ) ;
#3073 = CARTESIAN_POINT ( 'NONE',  ( 13.89598863503046111, -8.731428362939032795, 44.78571428571428470 ) ) ;
#3074 = FILL_AREA_STYLE ('',( #4684 ) ) ;
#3075 = CARTESIAN_POINT ( 'NONE',  ( -11.69682198916834892, -11.51250119794901394, 20.50404056962644006 ) ) ;
#3076 = CARTESIAN_POINT ( 'NONE',  ( -8.731428362939189114, 13.89598863503036341, 24.21428571428571530 ) ) ;
#3077 = PLANE ( 'NONE',  #6439 ) ;
#3078 = ORIENTED_EDGE ( 'NONE', *, *, #4094, .F. ) ;
#3079 = CARTESIAN_POINT ( 'NONE',  ( -11.60466159355861926, -11.60466159355875249, 4.500000000000005329 ) ) ;
#3080 = ADVANCED_FACE ( 'NONE', ( #9334 ), #2244, .T. ) ;
#3081 = CARTESIAN_POINT ( 'NONE',  ( -5.284464991282755264, 15.10213328493384743, 42.42857142857143060 ) ) ;
#3082 = AXIS2_PLACEMENT_3D ( 'NONE', #5180, #5837, #1247 ) ;
#3083 = CARTESIAN_POINT ( 'NONE',  ( 5.056896391392317724, -9.814260835640970626, 8.648862081921430800 ) ) ;
#3084 = CARTESIAN_POINT ( 'NONE',  ( -8.512513224245306986, -13.54758718765259218, 4.285714285714288252 ) ) ;
#3085 = CARTESIAN_POINT ( 'NONE',  ( 14.26974319298268767, -1.607813917172876472, 44.35714285714286831 ) ) ;
#3086 =( REPRESENTATION_RELATIONSHIP ('NONE','NONE', #58, #6629 ) REPRESENTATION_RELATIONSHIP_WITH_TRANSFORMATION ( #10068 )SHAPE_REPRESENTATION_RELATIONSHIP( ) );
#3087 = CARTESIAN_POINT ( 'NONE',  ( -13.59724543428031573, -4.619798703722008959, 38.93261199819787777 ) ) ;
#3088 = CARTESIAN_POINT ( 'NONE',  ( -9.383039235653820143, 1.486127417882155521, 5.700000000000038369 ) ) ;
#3089 = COLOUR_RGB ( '', 0.09019608, 0.27058824, 0.51372549) ;
#3090 = CARTESIAN_POINT ( 'NONE',  ( -7.806708723663830618, -7.806708723663901672, 17.25000000000003553 ) ) ;
#3091 = ORIENTED_EDGE ( 'NONE', *, *, #3345, .T. ) ;
#3092 = CARTESIAN_POINT ( 'NONE',  ( -13.89774397934249706, -1.693770420379375974, 43.13881657323070584 ) ) ;
#3093 = VERTEX_POINT ( 'NONE', #9738 ) ;
#3094 = CYLINDRICAL_SURFACE ( 'NONE', #3255, 1.649999999999984812 ) ;
#3095 = CARTESIAN_POINT ( 'NONE',  ( -11.51250119794888072, -11.69682198916848037, 18.49595943037356705 ) ) ;
#3096 = CARTESIAN_POINT ( 'NONE',  ( -1.791431617652833763, -15.89939535829188877, 9.857142857142855874 ) ) ;
#3097 = CARTESIAN_POINT ( 'NONE',  ( 1.513077731352925115, 9.873755945037100190, 13.44886208192141197 ) ) ;
#3098 = CARTESIAN_POINT ( 'NONE',  ( 15.88516839912898071, 1.917699372586004092, 28.13881657323070939 ) ) ;
#3099 = DIRECTION ( 'NONE',  ( 0.000000000000000000, 0.000000000000000000, 1.000000000000000000 ) ) ;
#3100 = CARTESIAN_POINT ( 'NONE',  ( 7.806708723663831506, 7.806708723663931870, 3.749999999999997335 ) ) ;
#3101 = DIRECTION ( 'NONE',  ( -1.000000000000000000, -0.000000000000000000, -0.000000000000000000 ) ) ;
#3102 = FILL_AREA_STYLE ('',( #10087 ) ) ;
#3103 =( GEOMETRIC_REPRESENTATION_CONTEXT ( 3 ) GLOBAL_UNCERTAINTY_ASSIGNED_CONTEXT ( ( #6479 ) ) GLOBAL_UNIT_ASSIGNED_CONTEXT ( ( #5379, #9370, #4709 ) ) REPRESENTATION_CONTEXT ( 'NONE', 'WORKASPACE' ) );
#3104 = VERTEX_POINT ( 'NONE', #4823 ) ;
#3105 = CARTESIAN_POINT ( 'NONE',  ( 9.938986324564400121, 12.66818340422679157, 51.38745637415366474 ) ) ;
#3106 = CARTESIAN_POINT ( 'NONE',  ( -9.355568503977838901, -4.766900247265279944, 5.400000000000016342 ) ) ;
#3107 = CARTESIAN_POINT ( 'NONE',  ( -1.837501619626328297, 16.30827793483733856, 12.64285714285714235 ) ) ;
#3108 = CARTESIAN_POINT ( 'NONE',  ( 0.000000000000000000, 20.00000000000000000, 0.000000000000000000 ) ) ;
#3109 =( GEOMETRIC_REPRESENTATION_CONTEXT ( 3 ) GLOBAL_UNCERTAINTY_ASSIGNED_CONTEXT ( ( #7216 ) ) GLOBAL_UNIT_ASSIGNED_CONTEXT ( ( #620, #5163, #5105 ) ) REPRESENTATION_CONTEXT ( 'NONE', 'WORKASPACE' ) );
#3110 = CARTESIAN_POINT ( 'NONE',  ( -1.776620879821455556, -10.89658364409025637, 0.9511379180785689558 ) ) ;
#3111 = CARTESIAN_POINT ( 'NONE',  ( -1.439022436064386845, 9.390499931835535108, 8.301137918078554279 ) ) ;
#3112 = DIRECTION ( 'NONE',  ( 3.081487911019577365E-32, 0.4999999999999990008, -0.8660254037844391517 ) ) ;
#3113 = CARTESIAN_POINT ( 'NONE',  ( 7.529642458189280241, -12.22833218042435099, 1.218326283912148922 ) ) ;
#3114 = CARTESIAN_POINT ( 'NONE',  ( 9.899494936611718643, -9.899494936611608509, 45.00000000000000711 ) ) ;
#3115 = ORIENTED_EDGE ( 'NONE', *, *, #5908, .T. ) ;
#3116 = DIRECTION ( 'NONE',  ( -1.000000000000000000, 0.000000000000000000, 0.000000000000000000 ) ) ;
#3117 = CARTESIAN_POINT ( 'NONE',  ( -5.420364854931999155, -15.49051278174644253, 46.07142857142856940 ) ) ;
#3118 = DIRECTION ( 'NONE',  ( 1.000000000000000000, 4.755747939841215952E-17, -0.000000000000000000 ) ) ;
#3119 = CARTESIAN_POINT ( 'NONE',  ( 1.439022436064387511, -9.390499931835512015, 0.8011379180785925813 ) ) ;
#3120 = CARTESIAN_POINT ( 'NONE',  ( 9.383039235653818366, -1.486127417882130208, 1.200000000000034373 ) ) ;
#3121 = CARTESIAN_POINT ( 'NONE',  ( -11.31370849898482156, 11.31370849898469544, 36.00000000000000711 ) ) ;
#3122 = CARTESIAN_POINT ( 'NONE',  ( -168.0000000000000284, -13.00000000000000533, 1.592040838891559490E-15 ) ) ;
#3123 = CARTESIAN_POINT ( 'NONE',  ( 11.22385875690717683, -11.40355824106234373, 31.00404056962644006 ) ) ;
#3124 = DIRECTION ( 'NONE',  ( 0.000000000000000000, 1.000000000000000000, 0.000000000000000000 ) ) ;
#3125 = CARTESIAN_POINT ( 'NONE',  ( -8.621071003556675549, 13.96533075980314642, 28.21832628391215181 ) ) ;
#3126 = DIRECTION ( 'NONE',  ( -1.000000000000000000, 0.000000000000000000, 0.000000000000000000 ) ) ;
#3127 = VERTEX_POINT ( 'NONE', #6508 ) ;
#3128 = DIRECTION ( 'NONE',  ( -1.000000000000000000, 0.000000000000000000, 0.000000000000000000 ) ) ;
#3129 = EDGE_CURVE ( 'NONE', #7109, #6243, #9033, .T. ) ;
#3130 =( NAMED_UNIT ( * ) PLANE_ANGLE_UNIT ( ) SI_UNIT ( $, .RADIAN. ) );
#3131 = CARTESIAN_POINT ( 'NONE',  ( 1.689666864740335894, -10.36326688006721497, 11.79886208192143471 ) ) ;
#3132 = CARTESIAN_POINT ( 'NONE',  ( -1.837501619626328297, 16.30827793483733856, 18.64285714285715656 ) ) ;
#3133 = ITEM_DEFINED_TRANSFORMATION ( 'NONE', 'NONE', #799,  #3995 ) ;
#3134 = CARTESIAN_POINT ( 'NONE',  ( 10.15407889436379030, 10.15407889436390221, 37.50000000000001421 ) ) ;
#3135 = CARTESIAN_POINT ( 'NONE',  ( 13.17239914596754424, -4.743843029824685864, 36.57546914105501656 ) ) ;
#3136 = CARTESIAN_POINT ( 'NONE',  ( 6.717514421272239744, -6.717514421272154479, 13.50000000000001243 ) ) ;
#3137 = CARTESIAN_POINT ( 'NONE',  ( -1.677562661911643938, -10.91227292449344688, 2.948862081921438616 ) ) ;
#3138 = EDGE_LOOP ( 'NONE', ( #1959, #7031 ) ) ;
#3139 = CARTESIAN_POINT ( 'NONE',  ( 12.15899005565164792, -7.639999817571655250, 8.785714285714293581 ) ) ;
#3140 = VECTOR ( 'NONE', #2358, 1000.000000000000000 ) ;
#3141 = ORIENTED_EDGE ( 'NONE', *, *, #2251, .T. ) ;
#3142 = CIRCLE ( 'NONE', #8764, 3.500000000000000000 ) ;
#3143 = ADVANCED_FACE ( 'NONE', ( #2595, #5791 ), #3419, .T. ) ;
#3144 = CARTESIAN_POINT ( 'NONE',  ( -6.717514421272238856, 6.717514421272181124, 0.000000000000000000 ) ) ;
#3145 = CARTESIAN_POINT ( 'NONE',  ( -15.44746603149413922, -5.543385399275820191, 30.92453085894499765 ) ) ;
#3146 = CIRCLE ( 'NONE', #5278, 8.000000000000000000 ) ;
#3147 = CARTESIAN_POINT ( 'NONE',  ( 13.54758718765249803, 8.512513224245457977, 7.714285714285715301 ) ) ;
#3148 = CARTESIAN_POINT ( 'NONE',  ( 1.967016585148662289, -16.29368510291087091, 17.63881657323070939 ) ) ;
#3149 = FACE_BOUND ( 'NONE', #4435, .T. ) ;
#3150 = CARTESIAN_POINT ( 'NONE',  ( 1.727091770866550968, 10.90442828429186761, 6.449999999999969091 ) ) ;
#3151 = DIRECTION ( 'NONE',  ( 0.000000000000000000, 1.387778780781445676E-16, -1.000000000000000000 ) ) ;
#3152 = STYLED_ITEM ( 'NONE', ( #9506 ), #7057 ) ;
#3153 = AXIS2_PLACEMENT_3D ( 'NONE', #5901, #9077, #1988 ) ;
#3154 = AXIS2_PLACEMENT_3D ( 'NONE', #889, #2531, #2429 ) ;
#3155 =( NAMED_UNIT ( * ) SI_UNIT ( $, .STERADIAN. ) SOLID_ANGLE_UNIT ( ) );
#3156 = VERTEX_POINT ( 'NONE', #1678 ) ;
#3157 = CARTESIAN_POINT ( 'NONE',  ( -13.51115193377584589, -4.865839792409295761, 12.92453085894499587 ) ) ;
#3158 = CARTESIAN_POINT ( 'NONE',  ( -7.806708723663831506, -7.806708723663907001, 8.250000000000030198 ) ) ;
#3159 = CARTESIAN_POINT ( 'NONE',  ( 13.89598863503046111, -8.731428362939032795, 14.78571428571429358 ) ) ;
#3160 = LINE ( 'NONE', #6249, #1399 ) ;
#3161 =( GEOMETRIC_REPRESENTATION_CONTEXT ( 3 ) GLOBAL_UNCERTAINTY_ASSIGNED_CONTEXT ( ( #8141 ) ) GLOBAL_UNIT_ASSIGNED_CONTEXT ( ( #1268, #9235, #2097 ) ) REPRESENTATION_CONTEXT ( 'NONE', 'WORKASPACE' ) );
#3162 = CARTESIAN_POINT ( 'NONE',  ( -13.25633410266679313, 4.503970704919840529, 31.56738800180213644 ) ) ;
#3163 = CARTESIAN_POINT ( 'NONE',  ( 10.36326688006723984, -1.689666864740210883, 6.201137918078538647 ) ) ;
#3164 = CARTESIAN_POINT ( 'NONE',  ( 1.776620879821457333, 10.89658364409028124, -0.5488620819214271584 ) ) ;
#3165 = CARTESIAN_POINT ( 'NONE',  ( -43.00000000000002842, 9.020562075080090842E-17, 13.00000000000001421 ) ) ;
#3166 = CARTESIAN_POINT ( 'NONE',  ( 12.08964793087886314, -7.750357176954162597, 0.7897548553407187644 ) ) ;
#3167 = AXIS2_PLACEMENT_3D ( 'NONE', #9300, #4381, #6841 ) ;
#3168 = CARTESIAN_POINT ( 'NONE',  ( 12.08964793087886314, -7.750357176954162597, 18.78975485534072121 ) ) ;
#3169 = EDGE_LOOP ( 'NONE', ( #8751, #3311, #1032, #8588, #5554 ) ) ;
#3170 = AXIS2_PLACEMENT_3D ( 'NONE', #6388, #8888, #9567 ) ;
#3171 = CARTESIAN_POINT ( 'NONE',  ( 16.32287076676382043, -1.707986654103810897, 16.35310228751641759 ) ) ;
#3172 = CARTESIAN_POINT ( 'NONE',  ( 0.000000000000000000, 1.773042676681366281, 0.000000000000000000 ) ) ;
#3173 = ADVANCED_FACE ( 'NONE', ( #3269 ), #5737, .F. ) ;
#3174 = CARTESIAN_POINT ( 'NONE',  ( -5.284464991282755264, 15.10213328493384743, 42.42857142857143060 ) ) ;
#3175 = FACE_OUTER_BOUND ( 'NONE', #2673, .T. ) ;
#3176 = CARTESIAN_POINT ( 'NONE',  ( -1.925929944387235853E-31, -1.018491042385001544, -1.270000000000007123 ) ) ;
#3177 = CARTESIAN_POINT ( 'NONE',  ( -6.717514421272238856, 6.717514421272181124, 18.00000000000001421 ) ) ;
#3178 = CARTESIAN_POINT ( 'NONE',  ( 9.383039235653818366, -1.486127417882129986, 4.199999999999981526 ) ) ;
#3179 = CARTESIAN_POINT ( 'NONE',  ( -15.10213328493390961, 5.284464991282586510, 35.57142857142857650 ) ) ;
#3180 = DIRECTION ( 'NONE',  ( 0.000000000000000000, 8.191099868251448390E-34, 1.000000000000000000 ) ) ;
#3181 = FACE_OUTER_BOUND ( 'NONE', #5847, .T. ) ;
#3182 = CARTESIAN_POINT ( 'NONE',  ( -15.91362231745475597, -1.665163862720028254, 39.14689771248358596 ) ) ;
#3183 = EDGE_LOOP ( 'NONE', ( #115, #458, #8887, #6583 ) ) ;
#3184 = CARTESIAN_POINT ( 'NONE',  ( 11.31370849898482334, -11.31370849898469366, 21.00000000000000355 ) ) ;
#3185 = DIRECTION ( 'NONE',  ( 0.000000000000000000, 0.000000000000000000, 1.000000000000000000 ) ) ;
#3186 = AXIS2_PLACEMENT_3D ( 'NONE', #8225, #2131, #1974 ) ;
#3187 = FACE_OUTER_BOUND ( 'NONE', #2468, .T. ) ;
#3188 = DIRECTION ( 'NONE',  ( 0.000000000000000000, 1.000000000000000000, 0.000000000000000000 ) ) ;
#3189 = CARTESIAN_POINT ( 'NONE',  ( 0.000000000000000000, 0.000000000000000000, 0.000000000000000000 ) ) ;
#3190 = AXIS2_PLACEMENT_3D ( 'NONE', #5290, #5144, #8391 ) ;
#3191 = CARTESIAN_POINT ( 'NONE',  ( -1.689666864740335228, 10.36326688006722740, 4.298862081921427603 ) ) ;
#3192 = CARTESIAN_POINT ( 'NONE',  ( 8.884063115244108744, 10.93517402715751885, 47.39553751340654486 ) ) ;
#3193 = CARTESIAN_POINT ( 'NONE',  ( 13.54758718765249803, 8.512513224245457977, 19.71428571428571175 ) ) ;
#3194 = PRODUCT_CONTEXT ( 'NONE', #7122, 'mechanical' ) ;
#3195 = CARTESIAN_POINT ( 'NONE',  ( -13.91197093850538380, -1.567502665446387278, 35.14285714285713880 ) ) ;
#3196 = EDGE_CURVE ( 'NONE', #3268, #8978, #110, .T. ) ;
#3197 = CARTESIAN_POINT ( 'NONE',  ( -12.08964793087886314, 7.750357176954159932, 33.78975485534073897 ) ) ;
#3198 = CARTESIAN_POINT ( 'NONE',  ( -1.562606840307830591, -9.865911304835490725, 4.950000000000017941 ) ) ;
#3199 = CARTESIAN_POINT ( 'NONE',  ( 7.424621202458790314, -7.424621202458697944, 13.50000000000001243 ) ) ;
#3200 = ORIENTED_EDGE ( 'NONE', *, *, #2564, .T. ) ;
#3201 = CARTESIAN_POINT ( 'NONE',  ( 8.684116361910502846, 11.09462624213450610, 51.38745637415366474 ) ) ;
#3202 = ORIENTED_EDGE ( 'NONE', *, *, #1783, .F. ) ;
#3203 = DIRECTION ( 'NONE',  ( 0.000000000000000000, 8.191099868251446680E-34, 1.000000000000000000 ) ) ;
#3204 = EDGE_CURVE ( 'NONE', #9396, #6730, #9685, .T. ) ;
#3205 = CARTESIAN_POINT ( 'NONE',  ( 11.31370849898482334, -11.31370849898469366, 15.00000000000000000 ) ) ;
#3206 = CARTESIAN_POINT ( 'NONE',  ( -8.404922754268618235, -13.61519076058357491, 18.28167371608785174 ) ) ;
#3207 = CARTESIAN_POINT ( 'NONE',  ( -4.766900247265192014, -9.355568503977876205, 2.099999999999990763 ) ) ;
#3208 = CARTESIAN_POINT ( 'NONE',  ( -1.642561882922479732, 10.37072757624895303, 0.2999999999999669598 ) ) ;
#3209 = PLANE ( 'NONE',  #9602 ) ;
#3210 = AXIS2_PLACEMENT_3D ( 'NONE', #6299, #1416, #8541 ) ;
#3211 = ORIENTED_EDGE ( 'NONE', *, *, #7111, .F. ) ;
#3212 = CARTESIAN_POINT ( 'NONE',  ( 4.743843029824831525, -13.17239914596749095, 17.42453085894499409 ) ) ;
#3213 = CARTESIAN_POINT ( 'NONE',  ( 9.837026868206070418, -5.012215536711392083, 13.34999999999998543 ) ) ;
#3214 = DIRECTION ( 'NONE',  ( -6.162975822039153635E-32, -0.5000000000000011102, -0.8660254037844379305 ) ) ;
#3215 = CARTESIAN_POINT ( 'NONE',  ( -10.06191849875405531, -10.24623928997363542, 24.49595943037356705 ) ) ;
#3216 = CARTESIAN_POINT ( 'NONE',  ( 1.595456901104624459, -10.37818827243064668, 0.8011379180785925813 ) ) ;
#3217 = CARTESIAN_POINT ( 'NONE',  ( 1.612135949262739398, 9.858066664633913234, 11.45113791807854220 ) ) ;
#3218 = LINE ( 'NONE', #4096, #2477 ) ;
#3219 = CARTESIAN_POINT ( 'NONE',  ( -9.809645194534070356, 9.989344678689256796, 4.004040569626432067 ) ) ;
#3220 = CARTESIAN_POINT ( 'NONE',  ( -4.865839792409144771, -13.51115193377589740, 14.07546914105500768 ) ) ;
#3221 = ORIENTED_EDGE ( 'NONE', *, *, #433, .T. ) ;
#3222 = CARTESIAN_POINT ( 'NONE',  ( 0.000000000000000000, -0.8865213383406761460, 1.535499999999911935 ) ) ;
#3223 = CARTESIAN_POINT ( 'NONE',  ( -11.31370849898482156, 11.31370849898469544, 48.00000000000000000 ) ) ;
#3224 = PLANE ( 'NONE',  #4494 ) ;
#3225 = DIRECTION ( 'NONE',  ( 0.000000000000000000, 6.338944243255235518E-49, -1.000000000000000000 ) ) ;
#3226 = CARTESIAN_POINT ( 'NONE',  ( 9.383039235653818366, -1.486127417882130208, 19.19999999999999574 ) ) ;
#3227 = CARTESIAN_POINT ( 'NONE',  ( -8.900167166472156666, 4.534861676072231340, 8.850000000000008527 ) ) ;
#3228 = CARTESIAN_POINT ( 'NONE',  ( -165.2818157524650360, 2.149893257473834307, 12.82099680185394242 ) ) ;
#3229 = CARTESIAN_POINT ( 'NONE',  ( -31.74999999999994316, 2.449293598294707893E-16, -2.000000000000000888 ) ) ;
#3230 = CARTESIAN_POINT ( 'NONE',  ( -15.06016580658428694, 5.404401153735006957, 39.57546914105500946 ) ) ;
#3231 = ORIENTED_EDGE ( 'NONE', *, *, #2126, .T. ) ;
#3232 = CARTESIAN_POINT ( 'NONE',  ( -15.89939535829186923, -1.791431617653016062, 35.14285714285713880 ) ) ;
#3233 = DIRECTION ( 'NONE',  ( -0.000000000000000000, -0.000000000000000000, -1.000000000000000000 ) ) ;
#3234 = CYLINDRICAL_SURFACE ( 'NONE', #7095, 18.00000000000000355 ) ;
#3235 = CARTESIAN_POINT ( 'NONE',  ( -88.00000000000002842, 0.000000000000000000, 13.00000000000000000 ) ) ;
#3236 = ADVANCED_FACE ( 'NONE', ( #1729 ), #8906, .F. ) ;
#3237 = DIRECTION ( 'NONE',  ( -1.000000000000000000, -0.000000000000000000, -0.000000000000000000 ) ) ;
#3238 = CARTESIAN_POINT ( 'NONE',  ( -5.056896391392315948, 9.814260835640991942, 13.14886208192146633 ) ) ;
#3239 = CARTESIAN_POINT ( 'NONE',  ( 1.689666864740335894, -10.36326688006720786, 14.79886208192143471 ) ) ;
#3240 = CARTESIAN_POINT ( 'NONE',  ( -11.92174236212692051, -7.340858601238089420, 44.71832628391215536 ) ) ;
#3241 = CARTESIAN_POINT ( 'NONE',  ( 15.89939535829187278, 1.791431617653015174, 14.14285714285714413 ) ) ;
#3242 = CARTESIAN_POINT ( 'NONE',  ( 7.639999817571788476, -12.15899005565156266, 39.21428571428571530 ) ) ;
#3243 = CARTESIAN_POINT ( 'NONE',  ( -7.556039541191334585, -11.78653521626503320, 44.28975485534073186 ) ) ;
#3244 = CARTESIAN_POINT ( 'NONE',  ( -12.15899005565164792, 7.639999817571651697, 5.785714285714282035 ) ) ;
#3245 = CARTESIAN_POINT ( 'NONE',  ( -108.0000000000000284, 0.000000000000000000, 0.000000000000000000 ) ) ;
#3246 = CARTESIAN_POINT ( 'NONE',  ( 4.766900247265192903, 9.355568503977902850, 18.60000000000000497 ) ) ;
#3247 = ORIENTED_EDGE ( 'NONE', *, *, #2438, .T. ) ;
#3248 = CARTESIAN_POINT ( 'NONE',  ( -13.91197093850538380, -1.567502665446387278, 5.142857142857143238 ) ) ;
#3249 = FACE_OUTER_BOUND ( 'NONE', #10102, .T. ) ;
#3250 = CARTESIAN_POINT ( 'NONE',  ( -11.31370849898482156, 11.31370849898469544, 18.00000000000000355 ) ) ;
#3251 = CARTESIAN_POINT ( 'NONE',  ( 13.96533075980324234, -8.621071003556521006, 34.78167371608785885 ) ) ;
#3252 = CARTESIAN_POINT ( 'NONE',  ( -9.355568503977838901, -4.766900247265279944, 11.39999999999996660 ) ) ;
#3253 = CARTESIAN_POINT ( 'NONE',  ( 9.355568503977840678, 4.766900247265305701, 6.899999999999961275 ) ) ;
#3254 = CARTESIAN_POINT ( 'NONE',  ( 11.85413878919593422, 7.448449071214774619, 1.714285714285716855 ) ) ;
#3255 = AXIS2_PLACEMENT_3D ( 'NONE', #8526, #3774, #6906 ) ;
#3256 = EDGE_LOOP ( 'NONE', ( #10227, #8788, #8586, #3337 ) ) ;
#3257 = CARTESIAN_POINT ( 'NONE',  ( 12.22833218042443271, -7.529642458189144349, 16.78167371608784819 ) ) ;
#3258 = CARTESIAN_POINT ( 'NONE',  ( -7.424621202458789426, 7.424621202458723701, 9.000000000000007105 ) ) ;
#3259 = CARTESIAN_POINT ( 'NONE',  ( -58.00000000000002842, 7.703719777548943412E-30, -1.059261469412979719E-30 ) ) ;
#3260 = CARTESIAN_POINT ( 'NONE',  ( -1.441234910513241818, -13.92619789766829008, 41.85310228751642825 ) ) ;
#3261 = CARTESIAN_POINT ( 'NONE',  ( 9.814260835641038128, -5.056896391392200485, 6.351137918078572753 ) ) ;
#3262 = CARTESIAN_POINT ( 'NONE',  ( -9.375578539472099848, 1.533232399700010351, 16.70113791807854398 ) ) ;
#3263 = PRESENTATION_LAYER_ASSIGNMENT (  '', '', ( #7732 ) ) ;
#3264 = DIRECTION ( 'NONE',  ( -1.000000000000000000, 0.000000000000000000, 0.000000000000000000 ) ) ;
#3265 = CARTESIAN_POINT ( 'NONE',  ( 1.478298951650704351, -14.28433602490913579, 7.646897712483577969 ) ) ;
#3266 =( LENGTH_UNIT ( ) NAMED_UNIT ( * ) SI_UNIT ( .MILLI., .METRE. ) );
#3267 = CARTESIAN_POINT ( 'NONE',  ( 12.08964793087886314, -7.750357176954162597, 6.789754855340717654 ) ) ;
#3268 = VERTEX_POINT ( 'NONE', #9587 ) ;
#3269 = FACE_OUTER_BOUND ( 'NONE', #2084, .T. ) ;
#3270 = CARTESIAN_POINT ( 'NONE',  ( 11.31370849898482334, -11.31370849898469366, 39.00000000000000000 ) ) ;
#3271 = CARTESIAN_POINT ( 'NONE',  ( -68.00000000000001421, 0.000000000000000000, 18.00000000000000355 ) ) ;
#3272 = DIRECTION ( 'NONE',  ( -1.000000000000000000, -1.387778780781445676E-16, -0.000000000000000000 ) ) ;
#3273 = CARTESIAN_POINT ( 'NONE',  ( 1.486127417882244783, -9.383039235653791721, 16.80000000000003624 ) ) ;
#3274 = CARTESIAN_POINT ( 'NONE',  ( 9.865911304835474738, 1.562606840307950051, 10.05000000000002736 ) ) ;
#3275 = FACE_OUTER_BOUND ( 'NONE', #3849, .T. ) ;
#3276 = CARTESIAN_POINT ( 'NONE',  ( 15.91362231745475597, 1.665163862720026255, 24.14689771248357530 ) ) ;
#3277 = DIRECTION ( 'NONE',  ( -1.000000000000000000, -0.000000000000000000, -0.000000000000000000 ) ) ;
#3278 = CARTESIAN_POINT ( 'NONE',  ( 11.69682198916835070, 11.51250119794901394, 35.50404056962644006 ) ) ;
#3279 = EDGE_LOOP ( 'NONE', ( #143, #4180 ) ) ;
#3280 = CARTESIAN_POINT ( 'NONE',  ( 5.420364854932001819, 15.49051278174644430, 25.07142857142858361 ) ) ;
#3281 = CARTESIAN_POINT ( 'NONE',  ( -11.48991645990274257, -11.34085470199651979, 0.000000000000000000 ) ) ;
#3282 = CARTESIAN_POINT ( 'NONE',  ( 13.54758718765249803, 8.512513224245457977, 1.714285714285716855 ) ) ;
#3283 = APPLICATION_CONTEXT ( 'automotive_design' ) ;
#3284 =( NAMED_UNIT ( * ) SI_UNIT ( $, .STERADIAN. ) SOLID_ANGLE_UNIT ( ) );
#3285 = CARTESIAN_POINT ( 'NONE',  ( 8.922933199037192509, -4.490180821391406951, 11.34886208192143364 ) ) ;
#3286 = CARTESIAN_POINT ( 'NONE',  ( -7.771249796623103556, -7.842167650704634063, 18.24886208192143044 ) ) ;
#3287 = UNCERTAINTY_MEASURE_WITH_UNIT (LENGTH_MEASURE( 1.000000000000000082E-05 ), #7007, 'distance_accuracy_value', 'NONE');
#3288 = CARTESIAN_POINT ( 'NONE',  ( 4.865839792409144771, 13.51115193377589740, 41.07546914105501656 ) ) ;
#3289 = CARTESIAN_POINT ( 'NONE',  ( -8.512513224245306986, -13.54758718765259218, 22.28571428571428470 ) ) ;
#3290 = CARTESIAN_POINT ( 'NONE',  ( 4.742819248065502258, 13.55419868402813499, 37.07142857142857650 ) ) ;
#3291 = CARTESIAN_POINT ( 'NONE',  ( -11.92174236212692051, -7.340858601238089420, 38.71832628391214826 ) ) ;
#3292 = EDGE_CURVE ( 'NONE', #9282, #6680, #10186, .T. ) ;
#3293 = CARTESIAN_POINT ( 'NONE',  ( -7.448449071214644945, -11.85413878919601771, 10.28571428571428648 ) ) ;
#3294 = DIRECTION ( 'NONE',  ( -1.000000000000000000, -0.000000000000000000, -0.000000000000000000 ) ) ;
#3295 = CARTESIAN_POINT ( 'NONE',  ( 1.677562661911645714, 10.91227292449347175, 10.44886208192141908 ) ) ;
#3296 = ORIENTED_EDGE ( 'NONE', *, *, #9611, .T. ) ;
#3297 = CARTESIAN_POINT ( 'NONE',  ( -13.25633410266679313, 4.503970704919840529, 49.56738800180214355 ) ) ;
#3298 = EDGE_CURVE ( 'NONE', #2212, #2369, #2495, .T. ) ;
#3299 = ORIENTED_EDGE ( 'NONE', *, *, #1473, .F. ) ;
#3300 = CARTESIAN_POINT ( 'NONE',  ( 2.000000000000001776, 0.8865213383407039016, -1.535500000000022958 ) ) ;
#3301 = EDGE_CURVE ( 'NONE', #94, #4710, #5720, .T. ) ;
#3302 = CARTESIAN_POINT ( 'NONE',  ( -15.10213328493390961, 5.284464991282586510, 11.57142857142857295 ) ) ;
#3303 = CIRCLE ( 'NONE', #9085, 3.632199999999998763 ) ;
#3304 = CARTESIAN_POINT ( 'NONE',  ( 8.841785722321695573, -13.82664651025757152, 35.21024514465927524 ) ) ;
#3305 = CARTESIAN_POINT ( 'NONE',  ( 10.90442828429183919, 1.727091770866679532, 13.04999999999999538 ) ) ;
#3306 = CARTESIAN_POINT ( 'NONE',  ( 1.727091770866550968, 10.90442828429187294, 9.449999999999988631 ) ) ;
#3307 = PLANE ( 'NONE',  #1013 ) ;
#3308 = FILL_AREA_STYLE ('',( #7028 ) ) ;
#3309 = CONICAL_SURFACE ( 'NONE', #5611, 1.535500000000000087, 1.047197551196590748 ) ;
#3310 = AXIS2_PLACEMENT_3D ( 'NONE', #10146, #8494, #1420 ) ;
#3311 = ORIENTED_EDGE ( 'NONE', *, *, #2389, .F. ) ;
#3312 = CARTESIAN_POINT ( 'NONE',  ( -9.989344678689363377, 9.809645194533960222, 19.99595943037356349 ) ) ;
#3313 = CARTESIAN_POINT ( 'NONE',  ( 5.012215536711512875, -9.837026868206002916, 10.65000000000001101 ) ) ;
#3314 = DIRECTION ( 'NONE',  ( -1.000000000000000000, 0.000000000000000000, 0.000000000000000000 ) ) ;
#3315 = CARTESIAN_POINT ( 'NONE',  ( -1.737328882695368115, 14.25515036105620581, 38.63881657323070584 ) ) ;
#3316 = CARTESIAN_POINT ( 'NONE',  ( -1.595456901104623348, 10.37818827243067155, 17.30113791807856316 ) ) ;
#3318 = AXIS2_PLACEMENT_3D ( 'NONE', #1370, #9952, #2033 ) ;
#3317 = CARTESIAN_POINT ( 'NONE',  ( -8.877401133907129704, 4.579542530753039742, 10.85113791807856209 ) ) ;
#3319 = AXIS2_PLACEMENT_3D ( 'NONE', #395, #8295, #5806 ) ;
#3320 = AXIS2_PLACEMENT_3D ( 'NONE', #1193, #3613, #2840 ) ;
#3321 = CARTESIAN_POINT ( 'NONE',  ( 6.717514421272239744, -6.717514421272154479, 19.50000000000001776 ) ) ;
#3322 = CARTESIAN_POINT ( 'NONE',  ( 7.529642458189280241, -12.22833218042435099, 19.21832628391215181 ) ) ;
#3323 = SURFACE_STYLE_USAGE ( .BOTH. , #8018 ) ;
#3324 = EDGE_CURVE ( 'NONE', #4862, #6875, #7042, .T. ) ;
#3325 = CARTESIAN_POINT ( 'NONE',  ( -13.17239914596754424, 4.743843029824683200, 9.575469141055007682 ) ) ;
#3326 = CARTESIAN_POINT ( 'NONE',  ( -58.00000000000001421, 2.204364238465235822E-15, -18.00000000000000355 ) ) ;
#3327 = COLOUR_RGB ( '', 0.72549020, 0.75294118, 0.79215686) ;
#3328 = CARTESIAN_POINT ( 'NONE',  ( 1.665163862719847732, 15.91362231745477374, 8.853102287516419366 ) ) ;
#3329 = CARTESIAN_POINT ( 'NONE',  ( -166.3194911921033849, -1.013757292147143385, 12.96131341066429954 ) ) ;
#3330 = CARTESIAN_POINT ( 'NONE',  ( -162.8500000000000512, -5.808233151972152598E-15, 15.00000000000000000 ) ) ;
#3331 = CARTESIAN_POINT ( 'NONE',  ( 9.873755945037075321, 1.513077731353043243, 9.051137918078573819 ) ) ;
#3332 = CARTESIAN_POINT ( 'NONE',  ( 1.486127417882244783, -9.383039235653782839, 10.80000000000003268 ) ) ;
#3333 = CARTESIAN_POINT ( 'NONE',  ( -166.7096159853958568, 1.311273010886724544, 12.93423035082597927 ) ) ;
#3334 = CARTESIAN_POINT ( 'NONE',  ( 1.707986654103998303, -16.32287076676380266, 31.64689771248358241 ) ) ;
#3335 = CARTESIAN_POINT ( 'NONE',  ( -6.717514421272238856, 6.717514421272181124, 2.585396704745767526E-18 ) ) ;
#3336 = CARTESIAN_POINT ( 'NONE',  ( -13.82664651025767100, 8.841785722321537477, 33.78975485534073897 ) ) ;
#3337 = ORIENTED_EDGE ( 'NONE', *, *, #8669, .F. ) ;
#3338 = CARTESIAN_POINT ( 'NONE',  ( 13.54758718765249803, 8.512513224245457977, 31.71428571428571530 ) ) ;
#3339 = DIRECTION ( 'NONE',  ( -1.000000000000000000, -0.000000000000000000, -0.000000000000000000 ) ) ;
#3340 = EDGE_CURVE ( 'NONE', #2833, #3031, #167, .T. ) ;
#3341 = CARTESIAN_POINT ( 'NONE',  ( -8.512513224245306986, -13.54758718765259218, 22.28571428571428470 ) ) ;
#3342 = FILL_AREA_STYLE_COLOUR ( '', #7114 ) ;
#3343 = CARTESIAN_POINT ( 'NONE',  ( -1.513077731352923339, -9.873755945037078874, 11.94886208192145993 ) ) ;
#3344 = CARTESIAN_POINT ( 'NONE',  ( 7.771249796623105333, 7.842167650704658932, 16.74886208192143755 ) ) ;
#3345 = EDGE_CURVE ( 'NONE', #2751, #5081, #9369, .T. ) ;
#3346 = CARTESIAN_POINT ( 'NONE',  ( 11.69682198916835070, 11.51250119794901394, -0.4959594303735606058 ) ) ;
#3347 = CARTESIAN_POINT ( 'NONE',  ( 5.284464991282756152, -15.10213328493384743, 15.42857142857143060 ) ) ;
#3348 = CARTESIAN_POINT ( 'NONE',  ( -4.742819248065500481, -13.55419868402813499, 46.07142857142857650 ) ) ;
#3349 = CARTESIAN_POINT ( 'NONE',  ( 13.17239914596754424, -4.743843029824685864, 36.57546914105501656 ) ) ;
#3350 = CARTESIAN_POINT ( 'NONE',  ( 13.91197093850538380, 1.567502665446386390, 14.14285714285714413 ) ) ;
#3351 = CARTESIAN_POINT ( 'NONE',  ( 8.900167166472158442, -4.534861676072210912, 19.34999999999997300 ) ) ;
#3352 = CARTESIAN_POINT ( 'NONE',  ( 4.724406229267374968, 9.377220287599064008, 7.598862081921438971 ) ) ;
#3353 = ORIENTED_EDGE ( 'NONE', *, *, #1311, .T. ) ;
#3354 = CARTESIAN_POINT ( 'NONE',  ( 13.55419868402807992, 4.742819248065648807, 7.928571428571430602 ) ) ;
#3355 = EDGE_LOOP ( 'NONE', ( #2455, #6488, #5967, #1576 ) ) ;
#3356 = FACE_OUTER_BOUND ( 'NONE', #1737, .T. ) ;
#3357 = CARTESIAN_POINT ( 'NONE',  ( -15.89939535829186923, -1.791431617653016062, 11.14285714285714235 ) ) ;
#3358 = CARTESIAN_POINT ( 'NONE',  ( -1.665163862719845067, -15.91362231745477374, 35.85310228751641404 ) ) ;
#3359 = CARTESIAN_POINT ( 'NONE',  ( -1.642561882922479732, 10.37072757624896191, 9.299999999999975842 ) ) ;
#3360 = CARTESIAN_POINT ( 'NONE',  ( -7.806708723663830618, -7.806708723663901672, 17.25000000000003553 ) ) ;
#3361 = CARTESIAN_POINT ( 'NONE',  ( -1.567502665446231180, -13.91197093850540334, 3.857142857142857650 ) ) ;
#3362 = CARTESIAN_POINT ( 'NONE',  ( 13.25633410266679313, -4.503970704919842305, 16.56738800180213289 ) ) ;
#3363 = CARTESIAN_POINT ( 'NONE',  ( 10.37072757624895836, -1.642561882922356498, 13.19999999999998863 ) ) ;
#3364 = CARTESIAN_POINT ( 'NONE',  ( -13.54758718765249625, -8.512513224245459753, 16.71428571428571530 ) ) ;
#3365 = CYLINDRICAL_SURFACE ( 'NONE', #9653, 16.00000000000000000 ) ;
#3366 = CARTESIAN_POINT ( 'NONE',  ( -13.89774397934249706, -1.693770420379375974, 43.13881657323070584 ) ) ;
#3367 = CARTESIAN_POINT ( 'NONE',  ( 4.967534682030706250, -9.859792900771036983, 15.65113791807858235 ) ) ;
#3368 = CARTESIAN_POINT ( 'NONE',  ( 4.490180821391514421, -8.922933199037132113, 15.65113791807858235 ) ) ;
#3369 = AXIS2_PLACEMENT_3D ( 'NONE', #8279, #1201, #8330 ) ;
#3370 = LINE ( 'NONE', #995, #6924 ) ;
#3371 = CARTESIAN_POINT ( 'NONE',  ( 11.92174236212692229, 7.340858601238088532, 23.71832628391215181 ) ) ;
#3372 = SURFACE_STYLE_USAGE ( .BOTH. , #6460 ) ;
#3373 = CARTESIAN_POINT ( 'NONE',  ( -1.478298951650703019, 14.28433602490913579, 16.64689771248358596 ) ) ;
#3374 = VERTEX_POINT ( 'NONE', #3326 ) ;
#3375 = CARTESIAN_POINT ( 'NONE',  ( -0.3021515714675195863, 13.99673906407701729, 48.73000000000003951 ) ) ;
#3376 = CARTESIAN_POINT ( 'NONE',  ( 13.47998361472151529, 8.620103694222146729, 15.71024514465927879 ) ) ;
#3377 = DIRECTION ( 'NONE',  ( -1.000000000000000000, -0.000000000000000000, -0.000000000000000000 ) ) ;
#3378 = CARTESIAN_POINT ( 'NONE',  ( -5.986002070941133901, -13.58603705635637304, -1.270000000000007123 ) ) ;
#3379 = CARTESIAN_POINT ( 'NONE',  ( 8.486213763410640709, 4.270415729527940130, 2.901137918078569466 ) ) ;
#3380 = CARTESIAN_POINT ( 'NONE',  ( -1.486127417882243895, 9.383039235653816590, 3.299999999999969624 ) ) ;
#3381 = CARTESIAN_POINT ( 'NONE',  ( -164.0468713975789115, 1.932340315393523023, 12.85570084551372183 ) ) ;
#3382 = CARTESIAN_POINT ( 'NONE',  ( -15.91362231745475597, -1.665163862720028254, 39.14689771248358596 ) ) ;
#3383 = CARTESIAN_POINT ( 'NONE',  ( 10.15407889436379030, 10.15407889436390576, 31.50000000000001421 ) ) ;
#3384 = CARTESIAN_POINT ( 'NONE',  ( 11.69682198916835070, 11.51250119794901394, 41.50404056962644006 ) ) ;
#3385 = VERTEX_POINT ( 'NONE', #3222 ) ;
#3386 = CARTESIAN_POINT ( 'NONE',  ( 16.30827793483735633, -1.837501619626142890, 32.35714285714286120 ) ) ;
#3387 = LINE ( 'NONE', #6568, #345 ) ;
#3388 = CARTESIAN_POINT ( 'NONE',  ( 11.60466159355862104, 11.60466159355875071, 13.50000000000000178 ) ) ;
#3389 = PLANE ( 'NONE',  #9926 ) ;
#3390 = CARTESIAN_POINT ( 'NONE',  ( -1.562606840307830591, -9.865911304835478290, 1.949999999999996181 ) ) ;
#3391 = CARTESIAN_POINT ( 'NONE',  ( 1.677562661911645714, 10.91227292449346642, 13.44886208192141197 ) ) ;
#3392 = CARTESIAN_POINT ( 'NONE',  ( 15.06016580658428694, -5.404401153735007846, 0.5754691410550027975 ) ) ;
#3393 = CARTESIAN_POINT ( 'NONE',  ( -8.512513224245306986, -13.54758718765259218, 34.28571428571428470 ) ) ;
#3394 = CARTESIAN_POINT ( 'NONE',  ( -166.6500000000000341, -1.532656754117495520E-15, 3.000000000000002665 ) ) ;
#3395 = CARTESIAN_POINT ( 'NONE',  ( 1.478298951650704351, -14.28433602490913579, 43.64689771248358596 ) ) ;
#3396 = CARTESIAN_POINT ( 'NONE',  ( -4.742819248065502258, -13.55419868402813677, 10.07142857142856940 ) ) ;
#3397 = CARTESIAN_POINT ( 'NONE',  ( -168.0000000000000284, -2.363368035607170010E-15, 0.000000000000000000 ) ) ;
#3398 = CARTESIAN_POINT ( 'NONE',  ( 1.677562661911645714, 10.91227292449346464, 4.448862081921434175 ) ) ;
#3399 = ORIENTED_EDGE ( 'NONE', *, *, #10144, .T. ) ;
#3400 = CARTESIAN_POINT ( 'NONE',  ( -7.448449071214644945, -11.85413878919601771, 22.28571428571428470 ) ) ;
#3401 = VERTEX_POINT ( 'NONE', #222 ) ;
#3402 = CARTESIAN_POINT ( 'NONE',  ( -2.000000000000001776, -9.511495879682425741E-17, 0.000000000000000000 ) ) ;
#3403 = CARTESIAN_POINT ( 'NONE',  ( -11.60466159355861748, -11.60466159355874893, 16.50000000000000000 ) ) ;
#3404 = CARTESIAN_POINT ( 'NONE',  ( -8.841785722321695573, 13.82664651025757152, 32.21024514465928235 ) ) ;
#3405 = CARTESIAN_POINT ( 'NONE',  ( 10.37072757624895836, -1.642561882922355609, 10.19999999999998685 ) ) ;
#3406 = CARTESIAN_POINT ( 'NONE',  ( -7.424621202458789426, 7.424621202458724589, 18.00000000000001421 ) ) ;
#3407 = CARTESIAN_POINT ( 'NONE',  ( 12.15899005565164792, -7.639999817571654361, 8.785714285714290028 ) ) ;
#3408 = ORIENTED_EDGE ( 'NONE', *, *, #9933, .T. ) ;
#3409 = CARTESIAN_POINT ( 'NONE',  ( 14.28433602490915000, -1.478298951650544479, 22.35310228751642114 ) ) ;
#3410 = CARTESIAN_POINT ( 'NONE',  ( -8.787954181158717404, -8.913453481710840620, -1.270000000000007123 ) ) ;
#3411 = CARTESIAN_POINT ( 'NONE',  ( -164.1695521934695989, 1.441888585351695395, 12.92005519273647707 ) ) ;
#3412 = CARTESIAN_POINT ( 'NONE',  ( 13.25633410266679313, -4.503970704919842305, 34.56738800180213644 ) ) ;
#3413 = CARTESIAN_POINT ( 'NONE',  ( -7.424621202458789426, 7.424621202458724589, 0.000000000000000000 ) ) ;
#3414 = CARTESIAN_POINT ( 'NONE',  ( -9.814260835641038128, 5.056896391392221801, 7.851137918078569200 ) ) ;
#3415 = AXIS2_PLACEMENT_3D ( 'NONE', #7350, #5645, #7150 ) ;
#3416 = DIRECTION ( 'NONE',  ( 0.000000000000000000, 8.191099868251446680E-34, 1.000000000000000000 ) ) ;
#3417 = CARTESIAN_POINT ( 'NONE',  ( 4.503970704919991519, -13.25633410266674517, 25.43261199819786711 ) ) ;
#3418 = CARTESIAN_POINT ( 'NONE',  ( -9.837026868206066865, 5.012215536711413399, 8.850000000000008527 ) ) ;
#3419 = CYLINDRICAL_SURFACE ( 'NONE', #449, 13.00000000000000355 ) ;
#3420 = CARTESIAN_POINT ( 'NONE',  ( -11.51250119794888072, -11.69682198916848037, 6.495959430373559051 ) ) ;
#3421 = CARTESIAN_POINT ( 'NONE',  ( -166.6066941517921123, -0.4327006227615173839, 12.99431788236279139 ) ) ;
#3422 = CARTESIAN_POINT ( 'NONE',  ( -58.00000000000002132, 7.703719777548943412E-30, -1.059261469412979719E-30 ) ) ;
#3423 = CARTESIAN_POINT ( 'NONE',  ( 1.439022436064387511, -9.390499931835517344, 3.801137918078595135 ) ) ;
#3424 = CARTESIAN_POINT ( 'NONE',  ( -1.562606840307830591, -9.865911304835478290, 13.95000000000002593 ) ) ;
#3425 = FACE_OUTER_BOUND ( 'NONE', #690, .T. ) ;
#3426 = CARTESIAN_POINT ( 'NONE',  ( 15.91362231745475597, 1.665163862720026255, 36.14689771248357886 ) ) ;
#3427 = CARTESIAN_POINT ( 'NONE',  ( 1.567502665446232957, 13.91197093850540156, 24.85714285714285765 ) ) ;
#3428 = CARTESIAN_POINT ( 'NONE',  ( -1.607813917173034124, 14.26974319298267524, 42.64285714285715301 ) ) ;
#3429 = ORIENTED_EDGE ( 'NONE', *, *, #6679, .F. ) ;
#3430 = CARTESIAN_POINT ( 'NONE',  ( -15.10213328493390961, 5.284464991282586510, 29.57142857142857650 ) ) ;
#3431 = DIRECTION ( 'NONE',  ( -1.000000000000000000, 0.000000000000000000, 0.000000000000000000 ) ) ;
#3432 = CARTESIAN_POINT ( 'NONE',  ( -11.60466159355861926, -11.60466159355875249, 16.50000000000000000 ) ) ;
#3433 = PRODUCT ( 'spacer', 'spacer', '', ( #9046 ) ) ;
#3434 = SURFACE_STYLE_USAGE ( .BOTH. , #8922 ) ;
#3435 = CARTESIAN_POINT ( 'NONE',  ( -9.390499931835536884, 1.439022436064298249, 15.69886208192145816 ) ) ;
#3436 = CARTESIAN_POINT ( 'NONE',  ( 6.751237864895159646, -6.683790977649233689, 5.498862081921462419 ) ) ;
#3437 = CARTESIAN_POINT ( 'NONE',  ( -5.164528828830334817, 15.14410076328347543, 16.43261199819786356 ) ) ;
#3438 = CARTESIAN_POINT ( 'NONE',  ( -15.10213328493390961, 5.284464991282586510, 29.57142857142857650 ) ) ;
#3439 = CARTESIAN_POINT ( 'NONE',  ( 15.91362231745475597, 1.665163862720026255, 0.1468977124835755543 ) ) ;
#3440 = CARTESIAN_POINT ( 'NONE',  ( -1.607813917173034124, 14.26974319298267524, 6.642857142857143238 ) ) ;
#3441 = ADVANCED_FACE ( 'NONE', ( #952 ), #6360, .T. ) ;
#3442 = CARTESIAN_POINT ( 'NONE',  ( 6.717514421272239744, -6.717514421272154479, 19.50000000000001776 ) ) ;
#3443 = CARTESIAN_POINT ( 'NONE',  ( 1.689666864740335894, -10.36326688006720786, 8.798862081921429379 ) ) ;
#3444 = CARTESIAN_POINT ( 'NONE',  ( -1.567502665446231180, -13.91197093850540334, 21.85714285714286120 ) ) ;
#3445 = EDGE_LOOP ( 'NONE', ( #8575, #3826, #7606, #9478 ) ) ;
#3446 = CARTESIAN_POINT ( 'NONE',  ( 15.10213328493390783, -5.284464991282587398, 32.57142857142856940 ) ) ;
#3447 = CARTESIAN_POINT ( 'NONE',  ( -5.297344310588352201, -15.53355953199867301, 36.06738800180213644 ) ) ;
#3448 = CARTESIAN_POINT ( 'NONE',  ( 10.90442828429183919, 1.727091770866678422, 4.049999999999988276 ) ) ;
#3449 = CARTESIAN_POINT ( 'NONE',  ( 1.607813917173037899, -14.26974319298267169, 15.64285714285714235 ) ) ;
#3450 = EDGE_CURVE ( 'NONE', #5925, #8713, #8033, .T. ) ;
#3451 = ORIENTED_EDGE ( 'NONE', *, *, #5975, .F. ) ;
#3452 = CARTESIAN_POINT ( 'NONE',  ( -13.89774397934249706, -1.693770420379375974, 31.13881657323070939 ) ) ;
#3453 = STYLED_ITEM ( 'NONE', ( #5194 ), #254 ) ;
#3454 = ORIENTED_EDGE ( 'NONE', *, *, #4219, .F. ) ;
#3455 = CARTESIAN_POINT ( 'NONE',  ( 10.19143222367002366, 10.12210786732603474, 48.73000000000001819 ) ) ;
#3456 = CARTESIAN_POINT ( 'NONE',  ( -10.06191849875405531, -10.24623928997363542, 36.49595943037355994 ) ) ;
#3457 = CARTESIAN_POINT ( 'NONE',  ( 9.814260835641038128, -5.056896391392198709, 15.35113791807859229 ) ) ;
#3458 = CARTESIAN_POINT ( 'NONE',  ( 7.390897758835871301, -7.458344646081624063, 3.501137918078585987 ) ) ;
#3459 = EDGE_CURVE ( 'NONE', #6853, #7160, #7021, .T. ) ;
#3460 = DIRECTION ( 'NONE',  ( 0.000000000000000000, -6.338944243255235518E-49, 1.000000000000000000 ) ) ;
#3461 = CARTESIAN_POINT ( 'NONE',  ( -4.865839792409144771, -13.51115193377589740, 20.07546914105500591 ) ) ;
#3462 = VECTOR ( 'NONE', #8822, 1000.000000000000000 ) ;
#3463 = AXIS2_PLACEMENT_3D ( 'NONE', #2554, #909, #7928 ) ;
#3464 =( NAMED_UNIT ( * ) SI_UNIT ( $, .STERADIAN. ) SOLID_ANGLE_UNIT ( ) );
#3465 = CARTESIAN_POINT ( 'NONE',  ( -1.478298951650703019, 14.28433602490913579, 22.64689771248357530 ) ) ;
#3466 = CARTESIAN_POINT ( 'NONE',  ( -7.424621202458789426, 7.424621202458723701, 9.000000000000007105 ) ) ;
#3467 = CARTESIAN_POINT ( 'NONE',  ( -15.14410076328353227, 5.164528828830164287, 43.56738800180213644 ) ) ;
#3468 = VERTEX_POINT ( 'NONE', #2695 ) ;
#3469 = CARTESIAN_POINT ( 'NONE',  ( -11.25886268110355992, 10.92057193546596494, 48.72999999999974108 ) ) ;
#3470 = CARTESIAN_POINT ( 'NONE',  ( -15.88516839912898071, -1.917699372586004980, 7.138816573230711171 ) ) ;
#3471 = CARTESIAN_POINT ( 'NONE',  ( -165.7329923747223859, -1.482200427765804296, 12.91529434110542240 ) ) ;
#3472 = CARTESIAN_POINT ( 'NONE',  ( -158.0000000000000284, -18.00000000000001066, 0.000000000000000000 ) ) ;
#3473 = CIRCLE ( 'NONE', #9920, 15.99999999999999645 ) ;
#3474 = AXIS2_PLACEMENT_3D ( 'NONE', #7413, #341, #6621 ) ;
#3475 = CIRCLE ( 'NONE', #9266, 3.500000000000000000 ) ;
#3476 = CARTESIAN_POINT ( 'NONE',  ( 4.490180821391514421, -8.922933199037132113, 9.651137918078598332 ) ) ;
#3477 = CARTESIAN_POINT ( 'NONE',  ( -4.490180821391513533, 8.922933199037158758, -0.8488620819214613977 ) ) ;
#3478 = SHAPE_REPRESENTATION ( 'spacer', ( #3995 ), #6118 ) ;
#3479 = CARTESIAN_POINT ( 'NONE',  ( -167.0398489105598685, 0.6938099590080268886, 14.98451262434803688 ) ) ;
#3480 = CARTESIAN_POINT ( 'NONE',  ( 5.164528828830335705, -15.14410076328347543, 37.43261199819787066 ) ) ;
#3481 = CARTESIAN_POINT ( 'NONE',  ( -12.15899005565164792, 7.639999817571651697, 29.78571428571428825 ) ) ;
#3482 = ADVANCED_FACE ( 'NONE', ( #9886 ), #7451, .T. ) ;
#3483 = AXIS2_PLACEMENT_3D ( 'NONE', #188, #2565, #8874 ) ;
#3484 = CARTESIAN_POINT ( 'NONE',  ( -13.91197093850538380, -1.567502665446387278, 41.14285714285714590 ) ) ;
#3485 = EDGE_CURVE ( 'NONE', #4710, #94, #4574, .T. ) ;
#3486 = VERTEX_POINT ( 'NONE', #4612 ) ;
#3487 = CARTESIAN_POINT ( 'NONE',  ( -5.420364854931999155, -15.49051278174644253, 40.07142857142857650 ) ) ;
#3488 = CARTESIAN_POINT ( 'NONE',  ( 0.000000000000000000, 4.523427693460793966E-32, 0.000000000000000000 ) ) ;
#3489 = CARTESIAN_POINT ( 'NONE',  ( 8.512513224245308763, 13.54758718765259040, 13.28571428571429003 ) ) ;
#3490 = PRESENTATION_STYLE_ASSIGNMENT (( #966 ) ) ;
#3491 = CARTESIAN_POINT ( 'NONE',  ( 5.110041130070070992, -16.97680807127747826, -1.270000000000007123 ) ) ;
#3492 = CARTESIAN_POINT ( 'NONE',  ( -9.858066664633883036, -1.612135949262833323, 15.54886208192143293 ) ) ;
#3493 = CARTESIAN_POINT ( 'NONE',  ( -1.533232399700100057, 9.375578539472094519, 10.29886208192143293 ) ) ;
#3494 = PRODUCT_DEFINITION_CONTEXT ( 'detailed design', #4873, 'design' ) ;
#3495 = CARTESIAN_POINT ( 'NONE',  ( 8.621071003556677326, -13.96533075980314287, 7.218326283912148256 ) ) ;
#3496 = CARTESIAN_POINT ( 'NONE',  ( 1.791431617652837316, 15.89939535829188877, 24.85714285714285765 ) ) ;
#3497 = CARTESIAN_POINT ( 'NONE',  ( 15.91362231745475597, 1.665163862720026255, 6.146897712483580634 ) ) ;
#3498 =( BOUNDED_CURVE ( )  B_SPLINE_CURVE ( 2, ( #7707, #628, #1403, #6080, #731, #2327, #7071, #7022, #1558, #3927, #6233, #3776, #4704, #1502, #4502, #2994, #777, #8528, #6856, #680, #6908, #6137, #7654, #2180, #9313, #7852, #3719, #4604, #2226, #6186, #9362, #5372, #3829, #6967, #3879, #10129, #3147, #3045, #2274, #5421, #8578, #10028, #5476, #4655, #10180, #6287, #3096, #9472, #6236, #9413, #5260, #1709, #3357, #9568, #3302, #4182, #1654, #7332, #982, #4855, #7283, #255, #1802, #46, #7955, #2425, #9670, #6492, #207, #933, #3205, #6339, #2578, #2471, #7131, #4078, #96, #3403, #8844, #6538, #5525, #9519, #5721, #8791, #3250, #4757, #6444, #5571, #148, #7228, #6390, #2374, #8684, #4804, #5625, #1606, #8890, #7901, #8734, #4956, #4130, #884, #4035, #4906, #8109, #825, #1038, #3982, #7180, #8003, #9624, #2526, #1755, #5676, #8052, #5208, #2722, #1087, #1953, #7583, #2825, #8943, #7428, #3654, #2622, #5970, #359, #8310, #5160, #5006, #9718, #9771, #5767, #409, #6731, #9919, #6636, #3599, #9148, #7379, #4437, #2055, #8358, #8153, #1278, #506, #1856, #2674, #4228, #5917, #305, #4278, #3446, #5865, #6586, #5102, #5820, #8997, #1906, #5055, #3553, #8201, #1133, #3506, #1231, #4382, #9820, #9043, #8252, #1181, #6681, #4330, #7481, #9865, #2770, #9091, #2006, #7533, #460, #4639, #2259, #1543, #4689, #7696, #9197, #560, #6069, #10166, #6018, #2977, #9243, #7746, #665, #6896, #10064, #9301, #5407, #2215, #3081, #6126, #5361, #6224, #10014, #8406, #7006, #2161, #8515, #7837, #1439, #5459, #6174, #4592, #1389, #3816, #7798, #3762, #6953, #8621, #5307, #764, #8564, #1488, #8464, #718, #3865, #4542, #615, #10118, #9401 ),
 .UNSPECIFIED., .F., .F. ) 
 B_SPLINE_CURVE_WITH_KNOTS ( ( 3, 2, 2, 2, 2, 2, 2, 2, 2, 2, 2, 2, 2, 2, 2, 2, 2, 2, 2, 2, 2, 2, 2, 2, 2, 2, 2, 2, 2, 2, 2, 2, 2, 2, 2, 2, 2, 2, 2, 2, 2, 2, 2, 2, 2, 2, 2, 2, 2, 2, 2, 2, 2, 2, 2, 2, 2, 2, 2, 2, 2, 2, 2, 2, 2, 2, 2, 2, 2, 2, 2, 2, 2, 2, 2, 2, 2, 2, 2, 2, 2, 2, 2, 2, 2, 2, 2, 2, 2, 2, 2, 2, 2, 2, 2, 2, 2, 2, 2, 2, 2, 2, 2, 2, 2, 2, 2, 2, 2, 2, 2, 2, 2, 2, 3 ),
 ( 0.000000000000000000, 0.007936507936507936067, 0.01587301587301587213, 0.02380952380952380820, 0.03174603174603174427, 0.03968253968253968728, 0.04761904761904761640, 0.05555555555555555247, 0.06349206349206348854, 0.07142857142857142461, 0.07936507936507937455, 0.08730158730158729674, 0.09523809523809523281, 0.1031746031746031828, 0.1111111111111111049, 0.1190476190476190410, 0.1269841269841269771, 0.1349206349206349131, 0.1428571428571428492, 0.1507936507936507853, 0.1587301587301587491, 0.1666666666666666574, 0.1746031746031745935, 0.1825396825396825295, 0.1904761904761904656, 0.1984126984126984017, 0.2063492063492063655, 0.2142857142857142738, 0.2222222222222222099, 0.2301587301587301460, 0.2380952380952380820, 0.2460317460317460181, 0.2539682539682539542, 0.2619047619047619180, 0.2698412698412698263, 0.2777777777777777901, 0.2857142857142856984, 0.2936507936507936622, 0.3015873015873015706, 0.3095238095238095344, 0.3174603174603174982, 0.3253968253968254065, 0.3333333333333333148, 0.3412698412698412787, 0.3492063492063491870, 0.3571428571428571508, 0.3650793650793650591, 0.3730158730158730229, 0.3809523809523809312, 0.3888888888888888951, 0.3968253968253968034, 0.4047619047619047672, 0.4126984126984127310, 0.4206349206349206393, 0.4285714285714285476, 0.4365079365079365115, 0.4444444444444444198, 0.4523809523809524391, 0.4603174603174602919, 0.4682539682539682557, 0.4761904761904761640, 0.4841269841269841279, 0.4920634920634920362, 0.5000000000000000000, 0.5079365079365079083, 0.5158730158730159276, 0.5238095238095238360, 0.5317460317460317443, 0.5396825396825396526, 0.5476190476190476719, 0.5555555555555555802, 0.5634920634920634885, 0.5714285714285713969, 0.5793650793650794162, 0.5873015873015873245, 0.5952380952380951218, 0.6031746031746031411, 0.6111111111111111605, 0.6190476190476190688, 0.6269841269841269771, 0.6349206349206349964, 0.6428571428571429047, 0.6507936507936508130, 0.6587301587301587213, 0.6666666666666666297, 0.6746031746031745380, 0.6825396825396825573, 0.6904761904761904656, 0.6984126984126983739, 0.7063492063492063933, 0.7142857142857143016, 0.7222222222222222099, 0.7301587301587301182, 0.7380952380952381375, 0.7460317460317460458, 0.7539682539682539542, 0.7619047619047618625, 0.7698412698412698818, 0.7777777777777777901, 0.7857142857142856984, 0.7936507936507936067, 0.8015873015873016261, 0.8095238095238095344, 0.8174603174603174427, 0.8253968253968254620, 0.8333333333333333703, 0.8412698412698412787, 0.8492063492063491870, 0.8571428571428570953, 0.8650793650793650036, 0.8730158730158730229, 0.8809523809523809312, 0.8888888888888888395, 0.8968253968253968589, 0.9023904529665212060 ),
 .UNSPECIFIED. ) 
 CURVE ( )  GEOMETRIC_REPRESENTATION_ITEM ( )  RATIONAL_B_SPLINE_CURVE ( ( 1.000000000000000000, 0.9749279121818236193, 1.000000000000000000, 0.9749279121818236193, 1.000000000000000000, 0.9749279121818236193, 1.000000000000000000, 0.9749279121818236193, 1.000000000000000000, 0.9749279121818236193, 1.000000000000000000, 0.9749279121818236193, 1.000000000000000000, 0.9749279121818236193, 1.000000000000000000, 0.9749279121818236193, 1.000000000000000000, 0.9749279121818236193, 1.000000000000000000, 0.9749279121818236193, 1.000000000000000000, 0.9749279121818236193, 1.000000000000000000, 0.9749279121818236193, 1.000000000000000000, 0.9749279121818236193, 1.000000000000000000, 0.9749279121818236193, 1.000000000000000000, 0.9749279121818236193, 1.000000000000000000, 0.9749279121818236193, 1.000000000000000000, 0.9749279121818236193, 1.000000000000000000, 0.9749279121818236193, 1.000000000000000000, 0.9749279121818236193, 1.000000000000000000, 0.9749279121818236193, 1.000000000000000000, 0.9749279121818236193, 1.000000000000000000, 0.9749279121818236193, 1.000000000000000000, 0.9749279121818236193, 1.000000000000000000, 0.9749279121818236193, 1.000000000000000000, 0.9749279121818236193, 1.000000000000000000, 0.9749279121818236193, 1.000000000000000000, 0.9749279121818236193, 1.000000000000000000, 0.9749279121818236193, 1.000000000000000000, 0.9749279121818236193, 1.000000000000000000, 0.9749279121818236193, 1.000000000000000000, 0.9749279121818236193, 1.000000000000000000, 0.9749279121818236193, 1.000000000000000000, 0.9749279121818236193, 1.000000000000000000, 0.9749279121818236193, 1.000000000000000000, 0.9749279121818236193, 1.000000000000000000, 0.9749279121818236193, 1.000000000000000000, 0.9749279121818236193, 1.000000000000000000, 0.9749279121818236193, 1.000000000000000000, 0.9749279121818236193, 1.000000000000000000, 0.9749279121818236193, 1.000000000000000000, 0.9749279121818236193, 1.000000000000000000, 0.9749279121818236193, 1.000000000000000000, 0.9749279121818236193, 1.000000000000000000, 0.9749279121818236193, 1.000000000000000000, 0.9749279121818236193, 1.000000000000000000, 0.9749279121818236193, 1.000000000000000000, 0.9749279121818236193, 1.000000000000000000, 0.9749279121818236193, 1.000000000000000000, 0.9749279121818236193, 1.000000000000000000, 0.9749279121818236193, 1.000000000000000000, 0.9749279121818236193, 1.000000000000000000, 0.9749279121818236193, 1.000000000000000000, 0.9749279121818236193, 1.000000000000000000, 0.9749279121818236193, 1.000000000000000000, 0.9749279121818236193, 1.000000000000000000, 0.9749279121818236193, 1.000000000000000000, 0.9749279121818236193, 1.000000000000000000, 0.9749279121818236193, 1.000000000000000000, 0.9749279121818236193, 1.000000000000000000, 0.9749279121818236193, 1.000000000000000000, 0.9749279121818236193, 1.000000000000000000, 0.9749279121818236193, 1.000000000000000000, 0.9749279121818236193, 1.000000000000000000, 0.9749279121818236193, 1.000000000000000000, 0.9749279121818236193, 1.000000000000000000, 0.9749279121818236193, 1.000000000000000000, 0.9749279121818236193, 1.000000000000000000, 0.9749279121818236193, 1.000000000000000000, 0.9749279121818236193, 1.000000000000000000, 0.9749279121818236193, 1.000000000000000000, 0.9749279121818236193, 1.000000000000000000, 0.9749279121818236193, 1.000000000000000000, 0.9749279121818236193, 1.000000000000000000, 0.9749279121818236193, 1.000000000000000000, 0.9749279121818236193, 1.000000000000000000, 0.9749279121818236193, 1.000000000000000000, 0.9749279121818236193, 1.000000000000000000, 0.9749279121818236193, 1.000000000000000000, 0.9749279121818236193, 1.000000000000000000, 0.9749279121818236193, 1.000000000000000000, 0.9749279121818236193, 1.000000000000000000, 0.9749279121818236193, 1.000000000000000000, 0.9749279121818236193, 1.000000000000000000, 0.9749279121818236193, 1.000000000000000000, 0.9749279121818236193, 1.000000000000000000, 0.9749279121818236193, 1.000000000000000000, 0.9749279121818236193, 1.000000000000000000, 0.9749279121818236193, 1.000000000000000000, 0.9749279121818236193, 1.000000000000000000, 0.9749279121818236193, 1.000000000000000000, 0.9749279121818236193, 1.000000000000000000, 0.9749279121818236193, 1.000000000000000000, 0.9749279121818236193, 1.000000000000000000, 0.9749279121818236193, 1.000000000000000000, 0.9749279121818236193, 1.000000000000000000, 0.9749279121818236193, 1.000000000000000000, 0.9749279121818236193, 1.000000000000000000, 0.9749279121818236193, 1.000000000000000000, 0.9749279121818236193, 1.000000000000000000, 0.9749279121818236193, 1.000000000000000000, 0.9749279121818236193, 1.000000000000000000, 0.9749279121818236193, 1.000000000000000000, 0.9749279121818236193, 1.000000000000000000, 0.9749279121818236193, 1.000000000000000000, 0.9749279121818236193, 1.000000000000000000, 0.9749279121818236193, 1.000000000000000000, 0.9749279121818236193, 1.000000000000000000, 0.9749279121818236193, 1.000000000000000000, 0.9749279121818236193, 1.000000000000000000, 0.9749279121818236193, 1.000000000000000000, 0.9749279121818236193, 1.000000000000000000, 0.9749279121818236193, 1.000000000000000000, 0.9749279121818236193, 1.000000000000000000, 0.9824195253882976875, 0.9894938054834325758 ) ) 
 REPRESENTATION_ITEM ( '' )  );
#3499 = CARTESIAN_POINT ( 'NONE',  ( 7.448449071214646722, 11.85413878919601594, 25.28571428571428470 ) ) ;
#3500 = CARTESIAN_POINT ( 'NONE',  ( 11.31370849898482334, -11.31370849898469366, 9.000000000000001776 ) ) ;
#3501 = CARTESIAN_POINT ( 'NONE',  ( 5.056896391392317724, -9.814260835640970626, 8.648862081921430800 ) ) ;
#3502 = EDGE_LOOP ( 'NONE', ( #9090, #6134 ) ) ;
#3503 = CARTESIAN_POINT ( 'NONE',  ( -14.26974319298268767, 1.607813917172874918, 11.35714285714285943 ) ) ;
#3504 = VECTOR ( 'NONE', #6827, 1000.000000000000114 ) ;
#3505 = ORIENTED_EDGE ( 'NONE', *, *, #1061, .T. ) ;
#3506 = CARTESIAN_POINT ( 'NONE',  ( -15.49051278174637858, -5.420364854932175014, 34.92857142857143771 ) ) ;
#3507 = CARTESIAN_POINT ( 'NONE',  ( 13.25633410266679313, -4.503970704919842305, 4.567388001802134667 ) ) ;
#3508 = CARTESIAN_POINT ( 'NONE',  ( 5.012215536711511987, -9.837026868205999364, 16.64999999999999858 ) ) ;
#3509 = EDGE_CURVE ( 'NONE', #5109, #1717, #3787, .T. ) ;
#3510 = CARTESIAN_POINT ( 'NONE',  ( -13.91197093850538380, -1.567502665446387278, 5.142857142857143238 ) ) ;
#3511 = EDGE_CURVE ( 'NONE', #1139, #879, #330, .T. ) ;
#3512 = CARTESIAN_POINT ( 'NONE',  ( 13.51115193377584589, 4.865839792409294873, 33.92453085894499054 ) ) ;
#3513 = ORIENTED_EDGE ( 'NONE', *, *, #4691, .F. ) ;
#3514 = SURFACE_SIDE_STYLE ('',( #2728 ) ) ;
#3515 = CIRCLE ( 'NONE', #8303, 2.200000000000001066 ) ;
#3516 = CARTESIAN_POINT ( 'NONE',  ( -16.00000000000000000, 0.000000000000000000, 113.2548339959390518 ) ) ;
#3517 = CARTESIAN_POINT ( 'NONE',  ( -9.858066664633883036, -1.612135949262833323, 3.548862081921419609 ) ) ;
#3518 = CARTESIAN_POINT ( 'NONE',  ( 4.619798703721856192, 13.59724543428036725, 51.06738800180214355 ) ) ;
#3519 = CARTESIAN_POINT ( 'NONE',  ( -1.776620879821455556, -10.89658364409025637, 15.95113791807857595 ) ) ;
#3520 = CARTESIAN_POINT ( 'NONE',  ( -4.809394265263009061, -9.333916720356718599, 1.101137918078559208 ) ) ;
#3521 = CIRCLE ( 'NONE', #2207, 3.500000000000000000 ) ;
#3522 = DIRECTION ( 'NONE',  ( -1.000000000000000000, 0.000000000000000000, 0.000000000000000000 ) ) ;
#3523 = CARTESIAN_POINT ( 'NONE',  ( -13.92619789766827054, -1.441234910513399470, 15.14689771248357708 ) ) ;
#3524 =( LENGTH_UNIT ( ) NAMED_UNIT ( * ) SI_UNIT ( .MILLI., .METRE. ) );
#3525 = PRODUCT ( 'spring hault', 'spring hault', '', ( #2725 ) ) ;
#3526 = CARTESIAN_POINT ( 'NONE',  ( 13.92619789766827587, 1.441234910513398582, 24.14689771248357530 ) ) ;
#3527 = CARTESIAN_POINT ( 'NONE',  ( -1.642561882922479732, 10.37072757624895303, 12.29999999999997762 ) ) ;
#3528 = CARTESIAN_POINT ( 'NONE',  ( 1.665163862719847732, 15.91362231745477374, 32.85310228751642114 ) ) ;
#3529 = CARTESIAN_POINT ( 'NONE',  ( -12.86099432095302575, 7.347572223948011683, 48.73000000000000398 ) ) ;
#3530 = CARTESIAN_POINT ( 'NONE',  ( -15.49051278174638036, -5.420364854932175902, 22.92857142857142705 ) ) ;
#3531 = CYLINDRICAL_SURFACE ( 'NONE', #7647, 18.00000000000000355 ) ;
#3532 = AXIS2_PLACEMENT_3D ( 'NONE', #6919, #3314, #5731 ) ;
#3533 = CARTESIAN_POINT ( 'NONE',  ( -4.490180821391513533, 8.922933199037158758, 5.151137918078567246 ) ) ;
#3534 = CARTESIAN_POINT ( 'NONE',  ( 6.717514421272239744, -6.717514421272154479, 16.50000000000001421 ) ) ;
#3535 = CARTESIAN_POINT ( 'NONE',  ( -83.00000000000001421, 0.000000000000000000, 13.00000000000000000 ) ) ;
#3536 = CARTESIAN_POINT ( 'NONE',  ( -4.623906867372410190, 13.21436662431711895, 24.42857142857143060 ) ) ;
#3537 = CARTESIAN_POINT ( 'NONE',  ( 7.639999817571789364, -12.15899005565156266, 39.21428571428571530 ) ) ;
#3538 = ORIENTED_EDGE ( 'NONE', *, *, #5805, .F. ) ;
#3539 = CARTESIAN_POINT ( 'NONE',  ( -11.31370849898482156, 11.31370849898469544, 48.00000000000000000 ) ) ;
#3540 = LINE ( 'NONE', #8290, #6746 ) ;
#3541 = CARTESIAN_POINT ( 'NONE',  ( 15.49051278174638036, 5.420364854932175014, 13.92857142857143238 ) ) ;
#3542 = CARTESIAN_POINT ( 'NONE',  ( 9.390499931835536884, -1.439022436064272936, 17.19886208192146171 ) ) ;
#3543 = CARTESIAN_POINT ( 'NONE',  ( 1.533232399700100945, -9.375578539472067874, 8.798862081921429379 ) ) ;
#3544 = CARTESIAN_POINT ( 'NONE',  ( 5.164528828830335705, -15.14410076328347543, 7.432611998197861780 ) ) ;
#3545 = CARTESIAN_POINT ( 'NONE',  ( -15.89939535829186923, -1.791431617653016062, 23.14285714285714590 ) ) ;
#3546 = CARTESIAN_POINT ( 'NONE',  ( 8.620103694221997515, 13.47998361472160767, 11.28975485534071943 ) ) ;
#3547 = CARTESIAN_POINT ( 'NONE',  ( 11.85413878919593422, 7.448449071214774619, 25.71428571428571885 ) ) ;
#3548 = CARTESIAN_POINT ( 'NONE',  ( 2.000000000000001776, 1.257743384770009870E-33, 1.535500000000000087 ) ) ;
#3549 = FACE_OUTER_BOUND ( 'NONE', #1935, .T. ) ;
#3550 = VERTEX_POINT ( 'NONE', #5978 ) ;
#3551 = CARTESIAN_POINT ( 'NONE',  ( 11.85413878919593422, 7.448449071214774619, 13.71428571428571352 ) ) ;
#3552 = VERTEX_POINT ( 'NONE', #3608 ) ;
#3553 = CARTESIAN_POINT ( 'NONE',  ( -8.512513224245306986, -13.54758718765259218, 34.28571428571428470 ) ) ;
#3554 = CARTESIAN_POINT ( 'NONE',  ( -13.51115193377584589, -4.865839792409295761, 6.924530858944994982 ) ) ;
#3555 = CARTESIAN_POINT ( 'NONE',  ( 9.859792900771104485, -4.967534682030589011, 2.348862081921457623 ) ) ;
#3556 = SHAPE_DEFINITION_REPRESENTATION ( #6717, #8171 ) ;
#3557 = CARTESIAN_POINT ( 'NONE',  ( -11.85413878919593422, -7.448449071214776396, 4.714285714285712636 ) ) ;
#3558 = ORIENTED_EDGE ( 'NONE', *, *, #4366, .F. ) ;
#3559 = CARTESIAN_POINT ( 'NONE',  ( 1.441234910513245149, 13.92619789766829008, 20.85310228751641759 ) ) ;
#3560 = LINE ( 'NONE', #2729, #5992 ) ;
#3561 = CARTESIAN_POINT ( 'NONE',  ( -5.056896391392315948, 9.814260835640997271, 19.14886208192144679 ) ) ;
#3562 = CARTESIAN_POINT ( 'NONE',  ( 13.21436662431716869, -4.623906867372263640, 2.571428571428571619 ) ) ;
#3563 = CARTESIAN_POINT ( 'NONE',  ( -1.642561882922479732, 10.37072757624896191, 6.299999999999972289 ) ) ;
#3564 = CARTESIAN_POINT ( 'NONE',  ( -7.390897758835869524, 7.458344646081644491, 5.001137918078545574 ) ) ;
#3565 = CARTESIAN_POINT ( 'NONE',  ( -108.0000000000000426, 0.000000000000000000, 0.000000000000000000 ) ) ;
#3566 = CARTESIAN_POINT ( 'NONE',  ( 1.478298951650704351, -14.28433602490913579, 31.64689771248358241 ) ) ;
#3567 = EDGE_CURVE ( 'NONE', #1705, #2768, #8869, .T. ) ;
#3568 = CARTESIAN_POINT ( 'NONE',  ( 1.642561882922480621, -10.37072757624891750, 10.80000000000003268 ) ) ;
#3569 = CARTESIAN_POINT ( 'NONE',  ( -13.17001005284346249, 7.209383666200358753, 48.73000000000002530 ) ) ;
#3570 = CARTESIAN_POINT ( 'NONE',  ( -163.3500000000000796, -0.2182232076591351377, 13.00000000000000533 ) ) ;
#3571 = CARTESIAN_POINT ( 'NONE',  ( 1.737328882695370558, -14.25515036105620581, 11.63881657323070939 ) ) ;
#3572 = CARTESIAN_POINT ( 'NONE',  ( -8.877401133907129704, 4.579542530753042406, 13.85113791807855321 ) ) ;
#3573 = CARTESIAN_POINT ( 'NONE',  ( -9.865911304835474738, -1.562606840307925626, 11.54999999999998295 ) ) ;
#3574 = DIRECTION ( 'NONE',  ( 1.000000000000000000, 0.000000000000000000, 0.000000000000000000 ) ) ;
#3575 = CARTESIAN_POINT ( 'NONE',  ( -5.543385399275643444, -15.44746603149420494, 38.07546914105502367 ) ) ;
#3576 = CARTESIAN_POINT ( 'NONE',  ( -11.85413878919593422, -7.448449071214776396, 46.71428571428571530 ) ) ;
#3577 = PRODUCT_DEFINITION_SHAPE ( 'NONE', 'NONE',  #10235 ) ;
#3578 =( GEOMETRIC_REPRESENTATION_CONTEXT ( 3 ) GLOBAL_UNCERTAINTY_ASSIGNED_CONTEXT ( ( #813 ) ) GLOBAL_UNIT_ASSIGNED_CONTEXT ( ( #5110, #4336, #5926 ) ) REPRESENTATION_CONTEXT ( 'NONE', 'WORKASPACE' ) );
#3579 = CARTESIAN_POINT ( 'NONE',  ( 14.26974319298268767, -1.607813917172876916, 44.35714285714287541 ) ) ;
#3580 = ORIENTED_EDGE ( 'NONE', *, *, #9373, .F. ) ;
#3581 = CARTESIAN_POINT ( 'NONE',  ( 5.284464991282756152, -15.10213328493384743, 45.42857142857143060 ) ) ;
#3582 = CARTESIAN_POINT ( 'NONE',  ( -4.920110265629110025, 15.11696251504478106, 1.442806492371169420E-14 ) ) ;
#3583 = CARTESIAN_POINT ( 'NONE',  ( 13.54758718765249803, 8.512513224245457977, 31.71428571428571530 ) ) ;
#3584 = DIRECTION ( 'NONE',  ( 0.000000000000000000, -6.338944243255235518E-49, 1.000000000000000000 ) ) ;
#3585 = CARTESIAN_POINT ( 'NONE',  ( 1.562606840307832368, 9.865911304835510265, 0.4499999999999856337 ) ) ;
#3586 = CARTESIAN_POINT ( 'NONE',  ( 8.922933199037192509, -4.490180821391406951, 11.34886208192143364 ) ) ;
#3587 = UNCERTAINTY_MEASURE_WITH_UNIT (LENGTH_MEASURE( 1.000000000000000082E-05 ), #7262, 'distance_accuracy_value', 'NONE');
#3588 = CARTESIAN_POINT ( 'NONE',  ( -4.766900247265192014, -9.355568503977867323, 11.09999999999999787 ) ) ;
#3589 = CARTESIAN_POINT ( 'NONE',  ( 1.707986654103998303, -16.32287076676380266, 7.646897712483577969 ) ) ;
#3590 = CARTESIAN_POINT ( 'NONE',  ( -13.89598863503046111, 8.731428362939027465, 23.78571428571429536 ) ) ;
#3591 =( LENGTH_UNIT ( ) NAMED_UNIT ( * ) SI_UNIT ( .MILLI., .METRE. ) );
#3592 = CARTESIAN_POINT ( 'NONE',  ( -11.22385875690717327, 11.40355824106234550, 4.004040569626432067 ) ) ;
#3593 = CARTESIAN_POINT ( 'NONE',  ( 1.567502665446232957, 13.91197093850540156, 18.85714285714285765 ) ) ;
#3594 = CARTESIAN_POINT ( 'NONE',  ( -11.31370849898482156, 11.31370849898469544, 0.000000000000000000 ) ) ;
#3595 = CARTESIAN_POINT ( 'NONE',  ( -13.54758718765249625, -8.512513224245459753, 40.71428571428571530 ) ) ;
#3596 = ORIENTED_EDGE ( 'NONE', *, *, #3340, .T. ) ;
#3597 = CARTESIAN_POINT ( 'NONE',  ( 7.639999817571789364, -12.15899005565156266, 15.21428571428571530 ) ) ;
#3598 = ORIENTED_EDGE ( 'NONE', *, *, #1870, .F. ) ;
#3599 = CARTESIAN_POINT ( 'NONE',  ( -16.30827793483735988, 1.837501619626141558, 29.35714285714286120 ) ) ;
#3600 = CARTESIAN_POINT ( 'NONE',  ( -1.665163862719845067, -15.91362231745477374, 47.85310228751642114 ) ) ;
#3601 = CARTESIAN_POINT ( 'NONE',  ( -1.677562661911643938, -10.91227292449344688, 2.948862081921438616 ) ) ;
#3602 = PRODUCT_DEFINITION_SHAPE ( 'NONE', 'NONE',  #10164 ) ;
#3603 = CARTESIAN_POINT ( 'NONE',  ( -4.742819248065500481, -13.55419868402813499, 10.07142857142856940 ) ) ;
#3604 = EDGE_CURVE ( 'NONE', #9714, #3042, #4405, .T. ) ;
#3605 = MANIFOLD_SOLID_BREP ( 'Boss-Extrude1', #4495 ) ;
#3606 = CARTESIAN_POINT ( 'NONE',  ( 13.51115193377584589, 4.865839792409294873, 27.92453085894499054 ) ) ;
#3607 = ORIENTED_EDGE ( 'NONE', *, *, #6954, .F. ) ;
#3608 = CARTESIAN_POINT ( 'NONE',  ( 5.110041130070070992, -16.97680807127747826, -1.270000000000007123 ) ) ;
#3609 = CARTESIAN_POINT ( 'NONE',  ( -43.00000000000002842, 6.933347799794049071E-30, -9.629649721936179265E-31 ) ) ;
#3610 = CARTESIAN_POINT ( 'NONE',  ( -9.333916720356675967, -4.809394265263096990, 18.39886208192140771 ) ) ;
#3611 = CARTESIAN_POINT ( 'NONE',  ( 9.837026868206066865, -5.012215536711392083, 1.350000000000015188 ) ) ;
#3612 = CARTESIAN_POINT ( 'NONE',  ( 4.967534682030706250, -9.859792900771036983, 12.65113791807859123 ) ) ;
#3613 = DIRECTION ( 'NONE',  ( 1.000000000000000000, 4.755747939841215952E-17, -0.000000000000000000 ) ) ;
#3614 = CARTESIAN_POINT ( 'NONE',  ( -13.59724543428031573, -4.619798703722008959, 26.93261199819786356 ) ) ;
#3615 = CARTESIAN_POINT ( 'NONE',  ( 5.012215536711511987, -9.837026868205997587, 7.649999999999992362 ) ) ;
#3616 = CARTESIAN_POINT ( 'NONE',  ( 15.44746603149413922, 5.543385399275817527, 33.92453085894499054 ) ) ;
#3617 = CARTESIAN_POINT ( 'NONE',  ( -8.994172837283734623, 11.03823571387622415, 48.73000000000002530 ) ) ;
#3618 = CARTESIAN_POINT ( 'NONE',  ( 5.284464991282756152, -15.10213328493384743, 21.42857142857142705 ) ) ;
#3619 = FACE_OUTER_BOUND ( 'NONE', #808, .T. ) ;
#3620 = CARTESIAN_POINT ( 'NONE',  ( 7.750357176954296712, -12.08964793087877787, 17.21024514465927879 ) ) ;
#3621 = CARTESIAN_POINT ( 'NONE',  ( -1.612135949262737844, -9.858066664633888365, 12.95113791807858128 ) ) ;
#3623 = AXIS2_PLACEMENT_3D ( 'NONE', #3929, #7855, #3099 ) ;
#3622 = CARTESIAN_POINT ( 'NONE',  ( 1.486127417882244783, -9.383039235653791721, 13.80000000000003446 ) ) ;
#3624 = DIRECTION ( 'NONE',  ( 0.000000000000000000, 0.000000000000000000, -1.000000000000000000 ) ) ;
#3625 = CARTESIAN_POINT ( 'NONE',  ( -1.478298951650703019, 14.28433602490913579, -1.353102287516420921 ) ) ;
#3626 = EDGE_CURVE ( 'NONE', #8713, #6711, #3752, .T. ) ;
#3627 = CARTESIAN_POINT ( 'NONE',  ( -11.85413878919593422, -7.448449071214776396, 40.71428571428571530 ) ) ;
#3628 = VERTEX_POINT ( 'NONE', #1094 ) ;
#3629 = ADVANCED_BREP_SHAPE_REPRESENTATION ( '', ( #286, #3995 ), #5470 ) ;
#3630 = VECTOR ( 'NONE', #6257, 1000.000000000000114 ) ;
#3631 = CARTESIAN_POINT ( 'NONE',  ( -13.54758718765249625, -8.512513224245459753, 40.71428571428571530 ) ) ;
#3632 = CIRCLE ( 'NONE', #9430, 1.816100000000000270 ) ;
#3633 = CARTESIAN_POINT ( 'NONE',  ( -2.358840667064915575, 15.62261993150980111, 1.394172777290095379E-15 ) ) ;
#3634 = VECTOR ( 'NONE', #8122, 1000.000000000000000 ) ;
#3635 = CARTESIAN_POINT ( 'NONE',  ( 1.791431617652837316, 15.89939535829188877, 24.85714285714285765 ) ) ;
#3636 = CARTESIAN_POINT ( 'NONE',  ( -58.00000000000001421, 0.000000000000000000, 18.00000000000000355 ) ) ;
#3637 = CARTESIAN_POINT ( 'NONE',  ( -9.355568503977838901, -4.766900247265280832, 2.400000000000013234 ) ) ;
#3638 = CARTESIAN_POINT ( 'NONE',  ( 1.486127417882244783, -9.383039235653782839, 7.800000000000029132 ) ) ;
#3639 = CARTESIAN_POINT ( 'NONE',  ( -8.922933199037192509, 4.490180821391424715, 6.848862081921446077 ) ) ;
#3640 = CARTESIAN_POINT ( 'NONE',  ( -5.012215536711506658, 9.837026868206022456, 18.15000000000000924 ) ) ;
#3641 = CARTESIAN_POINT ( 'NONE',  ( 8.621071003556677326, -13.96533075980314287, 13.21832628391215181 ) ) ;
#3642 = CARTESIAN_POINT ( 'NONE',  ( 16.30827793483735633, -1.837501619626142890, 44.35714285714287541 ) ) ;
#3643 = CIRCLE ( 'NONE', #2653, 15.00000000000000178 ) ;
#3644 = VECTOR ( 'NONE', #8007, 1000.000000000000000 ) ;
#3645 = CARTESIAN_POINT ( 'NONE',  ( -16.29368510291090288, 1.967016585148476215, 9.361183426769292382 ) ) ;
#3646 = ADVANCED_FACE ( 'NONE', ( #2630 ), #2681, .T. ) ;
#3647 = CARTESIAN_POINT ( 'NONE',  ( 12.15899005565164792, -7.639999817571655250, 20.78571428571429180 ) ) ;
#3648 = CARTESIAN_POINT ( 'NONE',  ( -8.512513224245306986, -13.54758718765259218, 10.28571428571428648 ) ) ;
#3649 = CARTESIAN_POINT ( 'NONE',  ( 10.03895970123120307, 12.58845729673829972, 49.39149694378009769 ) ) ;
#3650 = ORIENTED_EDGE ( 'NONE', *, *, #8828, .T. ) ;
#3651 = CARTESIAN_POINT ( 'NONE',  ( -5.012215536711506658, 9.837026868206022456, 18.15000000000000924 ) ) ;
#3652 = CARTESIAN_POINT ( 'NONE',  ( -165.0000000000000284, -6.071532165918824830E-15, 0.000000000000000000 ) ) ;
#3653 = STYLED_ITEM ( 'NONE', ( #4148 ), #3629 ) ;
#3654 = CARTESIAN_POINT ( 'NONE',  ( 16.30827793483735633, -1.837501619626142890, 26.35714285714286120 ) ) ;
#3655 = CARTESIAN_POINT ( 'NONE',  ( -11.51250119794888072, -11.69682198916848037, 48.49595943037355994 ) ) ;
#3656 = CARTESIAN_POINT ( 'NONE',  ( 7.806708723663831506, 7.806708723663925653, 15.74999999999996803 ) ) ;
#3657 = CARTESIAN_POINT ( 'NONE',  ( 5.284464991282756152, -15.10213328493384743, 3.428571428571426605 ) ) ;
#3658 = APPLICATION_PROTOCOL_DEFINITION ( 'draft international standard', 'automotive_design', 1998, #8367 ) ;
#3659 = CARTESIAN_POINT ( 'NONE',  ( 13.55419868402807992, 4.742819248065649695, 31.92857142857143060 ) ) ;
#3660 = CLOSED_SHELL ( 'NONE', ( #4316, #9400, #6703, #5314, #178, #6131, #7297, #8672, #8192, #2869, #5187, #1037, #9746 ) ) ;
#3661 = VECTOR ( 'NONE', #9518, 1000.000000000000000 ) ;
#3662 = CARTESIAN_POINT ( 'NONE',  ( -4.743843029824828861, 13.17239914596749450, 44.42453085894499765 ) ) ;
#3663 = ORIENTED_EDGE ( 'NONE', *, *, #716, .F. ) ;
#3664 = DIRECTION ( 'NONE',  ( 1.840628461782073167E-32, 6.938893903907220674E-18, 1.000000000000000000 ) ) ;
#3665 = CARTESIAN_POINT ( 'NONE',  ( 16.32287076676382043, -1.707986654103810897, 4.353102287516421143 ) ) ;
#3666 = CARTESIAN_POINT ( 'NONE',  ( 9.826155085340783302, 10.43469318297800896, 48.73000000000001819 ) ) ;
#3667 = PRODUCT_DEFINITION_SHAPE ( 'NONE', 'NONE',  #10232 ) ;
#3668 = CARTESIAN_POINT ( 'NONE',  ( -1.677562661911643938, -10.91227292449344688, 17.94886208192144395 ) ) ;
#3669 = EDGE_CURVE ( 'NONE', #2768, #9103, #8950, .T. ) ;
#3670 = CARTESIAN_POINT ( 'NONE',  ( -13.89774397934249706, -1.693770420379375974, 49.13881657323070584 ) ) ;
#3671 = CARTESIAN_POINT ( 'NONE',  ( -7.424621202458789426, 7.424621202458723701, 9.000000000000007105 ) ) ;
#3672 = CARTESIAN_POINT ( 'NONE',  ( 7.390897758835871301, -7.458344646081617846, 15.50113791807859620 ) ) ;
#3673 = CARTESIAN_POINT ( 'NONE',  ( -15.44569104238500046, -1.018491042384999545, -1.270000000000007123 ) ) ;
#3674 = CARTESIAN_POINT ( 'NONE',  ( -4.865839792409144771, -13.51115193377589740, 32.07546914105502367 ) ) ;
#3675 =( NAMED_UNIT ( * ) PLANE_ANGLE_UNIT ( ) SI_UNIT ( $, .RADIAN. ) );
#3676 = AXIS2_PLACEMENT_3D ( 'NONE', #3108, #7719, #639 ) ;
#3677 = CARTESIAN_POINT ( 'NONE',  ( 4.766900247265192903, 9.355568503977902850, 12.59999999999999964 ) ) ;
#3678 = CARTESIAN_POINT ( 'NONE',  ( 15.14410076328353227, -5.164528828830166063, 40.56738800180214355 ) ) ;
#3679 = CARTESIAN_POINT ( 'NONE',  ( -6.723343338700901839, 12.41960368482901700, 48.73000000000001819 ) ) ;
#3680 = CARTESIAN_POINT ( 'NONE',  ( 1.837501619626330074, -16.30827793483733501, 27.64285714285714590 ) ) ;
#3681 = CARTESIAN_POINT ( 'NONE',  ( 8.084771497730057628E-16, -16.99999999999997868, 2.081899558550498307E-15 ) ) ;
#3682 = CARTESIAN_POINT ( 'NONE',  ( -14.28433602490915000, 1.478298951650542481, 19.35310228751642825 ) ) ;
#3683 = CARTESIAN_POINT ( 'NONE',  ( 4.490180821391514421, -8.922933199037132113, 15.65113791807858235 ) ) ;
#3684 = CARTESIAN_POINT ( 'NONE',  ( 1.439022436064387511, -9.390499931835517344, 3.801137918078595135 ) ) ;
#3685 = CARTESIAN_POINT ( 'NONE',  ( -162.9598814269480158, 0.6930036797044089036, 14.98454961815950170 ) ) ;
#3686 = CARTESIAN_POINT ( 'NONE',  ( 8.620103694221997515, 13.47998361472160767, 41.28975485534072476 ) ) ;
#3687 = CARTESIAN_POINT ( 'NONE',  ( -13.21436662431716869, 4.623906867372262752, 47.57142857142857650 ) ) ;
#3688 = CARTESIAN_POINT ( 'NONE',  ( 1.478298951650704351, -14.28433602490913579, 1.646897712483578857 ) ) ;
#3689 = ORIENTED_EDGE ( 'NONE', *, *, #3204, .F. ) ;
#3690 = CARTESIAN_POINT ( 'NONE',  ( 8.731428362939190890, -13.89598863503036164, 45.21428571428572951 ) ) ;
#3691 = LINE ( 'NONE', #2086, #1824 ) ;
#3692 = CARTESIAN_POINT ( 'NONE',  ( 15.49051278174638036, 5.420364854932175014, 31.92857142857143415 ) ) ;
#3693 = DIRECTION ( 'NONE',  ( 0.000000000000000000, -6.338944243255235518E-49, 1.000000000000000000 ) ) ;
#3694 = DIRECTION ( 'NONE',  ( -1.000000000000000000, -0.000000000000000000, -0.000000000000000000 ) ) ;
#3695 = CARTESIAN_POINT ( 'NONE',  ( 9.383039235653818366, -1.486127417882129986, 10.19999999999998685 ) ) ;
#3696 = CARTESIAN_POINT ( 'NONE',  ( -4.579542530753125895, 8.877401133907090625, 19.14886208192144679 ) ) ;
#3697 = CARTESIAN_POINT ( 'NONE',  ( -9.355568503977838901, -4.766900247265279944, 17.39999999999997016 ) ) ;
#3698 = CARTESIAN_POINT ( 'NONE',  ( 11.69682198916835070, 11.51250119794901394, 17.50404056962643651 ) ) ;
#3699 = CARTESIAN_POINT ( 'NONE',  ( -15.10213328493390961, 5.284464991282586510, 47.57142857142857650 ) ) ;
#3700 = MANIFOLD_SOLID_BREP ( 'Revolve1', #3660 ) ;
#3701 = VECTOR ( 'NONE', #4141, 1000.000000000000000 ) ;
#3702 = CARTESIAN_POINT ( 'NONE',  ( 1.917699372585825790, 15.88516839912900203, 16.86118342676929061 ) ) ;
#3703 = CARTESIAN_POINT ( 'NONE',  ( -9.899494936611716867, 9.899494936611610285, 24.00000000000000000 ) ) ;
#3704 = CARTESIAN_POINT ( 'NONE',  ( 15.89939535829187278, 1.791431617653015174, 8.142857142857145902 ) ) ;
#3705 = CARTESIAN_POINT ( 'NONE',  ( 8.731428362939190890, -13.89598863503036164, 45.21428571428572951 ) ) ;
#3706 = ORIENTED_EDGE ( 'NONE', *, *, #2535, .F. ) ;
#3707 = CARTESIAN_POINT ( 'NONE',  ( -7.806708723663830618, -7.806708723663901672, 11.24999999999999467 ) ) ;
#3708 = ORIENTED_EDGE ( 'NONE', *, *, #9778, .F. ) ;
#3709 = CARTESIAN_POINT ( 'NONE',  ( -108.0000000000000426, -18.00000000000000355, 0.000000000000000000 ) ) ;
#3710 = CARTESIAN_POINT ( 'NONE',  ( 13.47998361472151529, 8.620103694222146729, 45.71024514465928235 ) ) ;
#3711 = CARTESIAN_POINT ( 'NONE',  ( 7.806708723663831506, 7.806708723663931870, 18.74999999999998934 ) ) ;
#3712 = CARTESIAN_POINT ( 'NONE',  ( -5.420364854931999155, -15.49051278174644253, 4.071428571428569398 ) ) ;
#3713 = CARTESIAN_POINT ( 'NONE',  ( -14.26974319298268767, 1.607813917172874696, 23.35714285714286120 ) ) ;
#3714 = EDGE_LOOP ( 'NONE', ( #6183, #10124 ) ) ;
#3715 = CARTESIAN_POINT ( 'NONE',  ( 14.28433602490915000, -1.478298951650544479, 46.35310228751641404 ) ) ;
#3716 = EDGE_LOOP ( 'NONE', ( #5589, #6654 ) ) ;
#3717 = CARTESIAN_POINT ( 'NONE',  ( -58.00000000000002132, 9.473114452887969885E-16, -8.200000000000001066 ) ) ;
#3718 = CARTESIAN_POINT ( 'NONE',  ( 8.841785722321695573, -13.82664651025757152, 29.21024514465927879 ) ) ;
#3719 = CARTESIAN_POINT ( 'NONE',  ( -15.10213328493390961, 5.284464991282586510, 5.571428571428574728 ) ) ;
#3720 = CARTESIAN_POINT ( 'NONE',  ( -1.533232399700100057, 9.375578539472094519, 1.298862081921425604 ) ) ;
#3721 = CARTESIAN_POINT ( 'NONE',  ( 8.684116361910502846, 11.09462624213450610, 51.38745637415366474 ) ) ;
#3722 = CARTESIAN_POINT ( 'NONE',  ( 5.012215536711511987, -9.837026868205997587, 7.649999999999992362 ) ) ;
#3723 = CARTESIAN_POINT ( 'NONE',  ( 4.809394265263009061, 9.333916720356739916, 17.60113791807856742 ) ) ;
#3724 = LINE ( 'NONE', #1459, #3819 ) ;
#3725 = CARTESIAN_POINT ( 'NONE',  ( -7.556039541191334585, -11.78653521626503320, 32.28975485534072476 ) ) ;
#3726 = VERTEX_POINT ( 'NONE', #1401 ) ;
#3727 = CARTESIAN_POINT ( 'NONE',  ( 7.458344646081711105, -7.390897758835786036, 2.498862081921459755 ) ) ;
#3728 = CARTESIAN_POINT ( 'NONE',  ( -15.44746603149413922, -5.543385399275820191, 48.92453085894499054 ) ) ;
#3729 = CARTESIAN_POINT ( 'NONE',  ( 10.90442828429184274, 1.727091770866679088, 7.050000000000010481 ) ) ;
#3730 = CARTESIAN_POINT ( 'NONE',  ( -15.49051278174638036, -5.420364854932175902, 28.92857142857143771 ) ) ;
#3731 = FACE_BOUND ( 'NONE', #1131, .T. ) ;
#3732 = CARTESIAN_POINT ( 'NONE',  ( 1.441234910513245149, 13.92619789766829008, 20.85310228751641759 ) ) ;
#3733 = CARTESIAN_POINT ( 'NONE',  ( 9.377220287599001836, 4.724406229267489543, -0.09886208192143307316 ) ) ;
#3734 = CARTESIAN_POINT ( 'NONE',  ( 1.612135949262739398, 9.858066664633913234, 8.451137918078549305 ) ) ;
#3735 = DIRECTION ( 'NONE',  ( 0.000000000000000000, -1.000000000000000000, 0.000000000000000000 ) ) ;
#3736 = CARTESIAN_POINT ( 'NONE',  ( 11.22385875690717683, -11.40355824106234373, 43.00404056962644717 ) ) ;
#3737 = CARTESIAN_POINT ( 'NONE',  ( -10.15407889436378852, -10.15407889436390576, 46.50000000000002132 ) ) ;
#3738 = EDGE_CURVE ( 'NONE', #1717, #273, #5826, .T. ) ;
#3739 = CARTESIAN_POINT ( 'NONE',  ( -4.623906867372410190, 13.21436662431711895, 48.42857142857143060 ) ) ;
#3740 = EDGE_LOOP ( 'NONE', ( #1982, #8387 ) ) ;
#3741 = CARTESIAN_POINT ( 'NONE',  ( 11.40355824106246985, -11.22385875690704538, 4.995959430373563492 ) ) ;
#3742 = DIRECTION ( 'NONE',  ( -6.162975822039153635E-32, -0.5000000000000011102, -0.8660254037844379305 ) ) ;
#3743 = CARTESIAN_POINT ( 'NONE',  ( -1.837501619626328297, 16.30827793483733856, 36.64285714285714590 ) ) ;
#3744 = CARTESIAN_POINT ( 'NONE',  ( -31.74999999999994316, 1.638219973650290020E-33, 2.000000000000000888 ) ) ;
#3745 = SURFACE_SIDE_STYLE ('',( #652 ) ) ;
#3746 = DIRECTION ( 'NONE',  ( -6.162975822039153635E-32, -0.5000000000000011102, -0.8660254037844379305 ) ) ;
#3747 = CARTESIAN_POINT ( 'NONE',  ( -1.562606840307830591, -9.865911304835478290, 10.95000000000000462 ) ) ;
#3748 = CARTESIAN_POINT ( 'NONE',  ( -8.442910196168309511, -4.355403765523546689, 15.39886208192141126 ) ) ;
#3749 = DIRECTION ( 'NONE',  ( 0.000000000000000000, 6.938893903907221444E-18, 1.000000000000000000 ) ) ;
#3750 = CARTESIAN_POINT ( 'NONE',  ( 13.82664651025767100, -8.841785722321541030, 18.78975485534072121 ) ) ;
#3751 = CARTESIAN_POINT ( 'NONE',  ( 1.837501619626330074, -16.30827793483733501, 45.64285714285716011 ) ) ;
#3752 = CIRCLE ( 'NONE', #9536, 3.632200000000000539 ) ;
#3753 = SURFACE_SIDE_STYLE ('',( #6946 ) ) ;
#3754 = CARTESIAN_POINT ( 'NONE',  ( 5.164528828830335705, -15.14410076328347543, 13.43261199819786711 ) ) ;
#3755 = ORIENTED_EDGE ( 'NONE', *, *, #6995, .T. ) ;
#3756 = CARTESIAN_POINT ( 'NONE',  ( 10.15407889436379030, 10.15407889436390576, 31.50000000000001421 ) ) ;
#3757 = CARTESIAN_POINT ( 'NONE',  ( -5.420364854931999155, -15.49051278174644253, 22.07142857142858006 ) ) ;
#3758 = CARTESIAN_POINT ( 'NONE',  ( 5.420364854932001819, 15.49051278174644430, 49.07142857142859071 ) ) ;
#3759 = EDGE_LOOP ( 'NONE', ( #4277, #8497 ) ) ;
#3760 = CARTESIAN_POINT ( 'NONE',  ( 7.424621202458790314, -7.424621202458697944, 13.50000000000001243 ) ) ;
#3761 = SURFACE_SIDE_STYLE ('',( #614 ) ) ;
#3762 = CARTESIAN_POINT ( 'NONE',  ( -5.420364854931998266, -15.49051278174643898, 46.07142857142857650 ) ) ;
#3763 = SURFACE_STYLE_FILL_AREA ( #666 ) ;
#3764 = CARTESIAN_POINT ( 'NONE',  ( 1.677562661911645714, 10.91227292449347175, 10.44886208192141908 ) ) ;
#3765 = CARTESIAN_POINT ( 'NONE',  ( 11.31370849898482334, -11.31370849898469366, 9.000000000000001776 ) ) ;
#3766 = CARTESIAN_POINT ( 'NONE',  ( 11.31370849898482334, -11.31370849898469366, 3.000000000000002665 ) ) ;
#3767 = CARTESIAN_POINT ( 'NONE',  ( 0.000000000000000000, 0.000000000000000000, 0.000000000000000000 ) ) ;
#3768 = CARTESIAN_POINT ( 'NONE',  ( -12.15899005565164792, 7.639999817571650809, 23.78571428571429180 ) ) ;
#3769 = ADVANCED_FACE ( 'NONE', ( #7652 ), #2272, .T. ) ;
#3770 = CARTESIAN_POINT ( 'NONE',  ( -9.809645194534070356, 9.989344678689256796, 22.00404056962643651 ) ) ;
#3771 = CARTESIAN_POINT ( 'NONE',  ( -9.989344678689363377, 9.809645194533960222, 43.99595943037355994 ) ) ;
#3772 = CARTESIAN_POINT ( 'NONE',  ( -1.642561882922479732, 10.37072757624896191, 6.299999999999972289 ) ) ;
#3773 = ORIENTED_EDGE ( 'NONE', *, *, #9018, .T. ) ;
#3774 = DIRECTION ( 'NONE',  ( -0.000000000000000000, -0.000000000000000000, 1.000000000000000000 ) ) ;
#3775 = CARTESIAN_POINT ( 'NONE',  ( 13.96533075980324234, -8.621071003556521006, 22.78167371608784464 ) ) ;
#3776 = CARTESIAN_POINT ( 'NONE',  ( 16.30827793483735633, -1.837501619626142890, 2.357142857142856762 ) ) ;
#3777 = CARTESIAN_POINT ( 'NONE',  ( -4.270415729527831772, -8.486213763410670907, 9.098862081921437195 ) ) ;
#3778 = CARTESIAN_POINT ( 'NONE',  ( 15.44746603149413922, 5.543385399275817527, 27.92453085894499054 ) ) ;
#3779 = CARTESIAN_POINT ( 'NONE',  ( 9.837026868206066865, -5.012215536711391195, 4.350000000000036948 ) ) ;
#3780 = CARTESIAN_POINT ( 'NONE',  ( 9.814260835641038128, -5.056896391392198709, 12.35113791807855677 ) ) ;
#3781 = CARTESIAN_POINT ( 'NONE',  ( -4.246973736992222470, -14.10948682827616096, -1.270000000000007123 ) ) ;
#3782 = CARTESIAN_POINT ( 'NONE',  ( -14.25515036105622890, 1.737328882695209575, 27.36118342676929416 ) ) ;
#3783 = ADVANCED_FACE ( 'NONE', ( #2116 ), #3827, .F. ) ;
#3784 = ORIENTED_EDGE ( 'NONE', *, *, #417, .F. ) ;
#3785 = PRODUCT_RELATED_PRODUCT_CATEGORY ( 'part', '', ( #6639 ) ) ;
#3786 = CARTESIAN_POINT ( 'NONE',  ( -14.28433602490915000, 1.478298951650542481, 7.353102287516419366 ) ) ;
#3787 = LINE ( 'NONE', #9424, #4904 ) ;
#3788 = DIRECTION ( 'NONE',  ( -0.5000000000000061062, 1.060575238724902601E-16, -0.8660254037844351549 ) ) ;
#3789 = EDGE_CURVE ( 'NONE', #2003, #9194, #2224, .T. ) ;
#3790 = CARTESIAN_POINT ( 'NONE',  ( 13.25633410266679313, -4.503970704919842305, 16.56738800180213289 ) ) ;
#3791 = CARTESIAN_POINT ( 'NONE',  ( 8.877401133907127928, -4.579542530753017537, 15.35113791807859229 ) ) ;
#3792 = CARTESIAN_POINT ( 'NONE',  ( 8.877401133907127928, -4.579542530753017537, 0.3511379180785880183 ) ) ;
#3793 = PLANE ( 'NONE',  #2969 ) ;
#3794 = CARTESIAN_POINT ( 'NONE',  ( 9.899494936611718643, -9.899494936611608509, 39.00000000000000000 ) ) ;
#3795 = CARTESIAN_POINT ( 'NONE',  ( 12.15899005565164792, -7.639999817571655250, 44.78571428571428470 ) ) ;
#3796 = ORIENTED_EDGE ( 'NONE', *, *, #8259, .T. ) ;
#3797 = CARTESIAN_POINT ( 'NONE',  ( -15.88516839912898071, -1.917699372586004980, 13.13881657323070584 ) ) ;
#3798 = CARTESIAN_POINT ( 'NONE',  ( -5.986002070941136566, -13.58603705635637482, -1.270000000000007123 ) ) ;
#3799 = CARTESIAN_POINT ( 'NONE',  ( -1.837501619626328297, 16.30827793483733856, 24.64285714285714235 ) ) ;
#3800 = FACE_BOUND ( 'NONE', #10074, .T. ) ;
#3801 =( GEOMETRIC_REPRESENTATION_CONTEXT ( 3 ) GLOBAL_UNCERTAINTY_ASSIGNED_CONTEXT ( ( #8778 ) ) GLOBAL_UNIT_ASSIGNED_CONTEXT ( ( #6881, #2859, #2808 ) ) REPRESENTATION_CONTEXT ( 'NONE', 'WORKASPACE' ) );
#3802 = DIRECTION ( 'NONE',  ( 0.000000000000000000, 0.000000000000000000, 1.000000000000000000 ) ) ;
#3803 = CARTESIAN_POINT ( 'NONE',  ( 8.900167166472154889, -4.534861676072210024, 4.350000000000036948 ) ) ;
#3804 = CARTESIAN_POINT ( 'NONE',  ( 1.533232399700100945, -9.375578539472067874, 14.79886208192143471 ) ) ;
#3805 = DIRECTION ( 'NONE',  ( 1.000000000000000000, 0.000000000000000000, 0.000000000000000000 ) ) ;
#3806 = CARTESIAN_POINT ( 'NONE',  ( -11.31370849898482156, 11.31370849898469544, 42.00000000000000000 ) ) ;
#3807 = CARTESIAN_POINT ( 'NONE',  ( -3.270000000000004459, -6.360255186938576580E-15, -6.143598522982476548E-16 ) ) ;
#3808 = CARTESIAN_POINT ( 'NONE',  ( 15.06016580658428694, -5.404401153735007846, 18.57546914105500235 ) ) ;
#3809 = AXIS2_PLACEMENT_3D ( 'NONE', #3984, #683, #1560 ) ;
#3810 = AXIS2_PLACEMENT_3D ( 'NONE', #6405, #4922, #2440 ) ;
#3811 = CARTESIAN_POINT ( 'NONE',  ( -15.89939535829186923, -1.791431617653016062, 23.14285714285714590 ) ) ;
#3812 = DIRECTION ( 'NONE',  ( 1.000000000000000000, 0.000000000000000000, 0.000000000000000000 ) ) ;
#3813 = ORIENTED_EDGE ( 'NONE', *, *, #9711, .T. ) ;
#3814 = CARTESIAN_POINT ( 'NONE',  ( -7.424621202458789426, 7.424621202458724589, 12.00000000000001066 ) ) ;
#3815 = ORIENTED_EDGE ( 'NONE', *, *, #1622, .T. ) ;
#3816 = CARTESIAN_POINT ( 'NONE',  ( 1.837501619626329630, -16.30827793483733501, 45.64285714285715301 ) ) ;
#3817 = CIRCLE ( 'NONE', #8926, 0.4999999999999994449 ) ;
#3818 = AXIS2_PLACEMENT_3D ( 'NONE', #1479, #600, #3802 ) ;
#3819 = VECTOR ( 'NONE', #2231, 1000.000000000000227 ) ;
#3820 = CARTESIAN_POINT ( 'NONE',  ( -10.37818827243067688, 1.595456901104523428, 9.698862081921454603 ) ) ;
#3821 = CARTESIAN_POINT ( 'NONE',  ( -5.420364854931999155, -15.49051278174644253, 4.071428571428569398 ) ) ;
#3822 = CARTESIAN_POINT ( 'NONE',  ( -8.731428362939189114, 13.89598863503036341, 6.214285714285717965 ) ) ;
#3823 = CARTESIAN_POINT ( 'NONE',  ( -4.742819248065500481, -13.55419868402813499, 28.07142857142857295 ) ) ;
#3824 = CARTESIAN_POINT ( 'NONE',  ( 6.717514421272239744, -6.717514421272154479, 10.50000000000000888 ) ) ;
#3825 = CARTESIAN_POINT ( 'NONE',  ( 13.25633410266679313, -4.503970704919842305, 46.56738800180214355 ) ) ;
#3826 = ORIENTED_EDGE ( 'NONE', *, *, #9652, .T. ) ;
#3827 = CYLINDRICAL_SURFACE ( 'NONE', #1933, 0.9906000000000003691 ) ;
#3828 = CARTESIAN_POINT ( 'NONE',  ( -13.47998361472151174, -8.620103694222146729, 24.71024514465928235 ) ) ;
#3829 = CARTESIAN_POINT ( 'NONE',  ( 1.791431617652837316, 15.89939535829188877, 6.857142857142860315 ) ) ;
#3830 = CARTESIAN_POINT ( 'NONE',  ( -8.922933199037192509, 4.490180821391428267, 12.84886208192143009 ) ) ;
#3831 = CARTESIAN_POINT ( 'NONE',  ( 1.665163862719847732, 15.91362231745477374, 20.85310228751641759 ) ) ;
#3832 = CARTESIAN_POINT ( 'NONE',  ( -5.012215536711506658, 9.837026868206027785, 0.1499999999999952482 ) ) ;
#3833 = CARTESIAN_POINT ( 'NONE',  ( -9.377220287598998283, -4.724406229267462898, 13.40113791807857702 ) ) ;
#3834 = DIRECTION ( 'NONE',  ( 0.000000000000000000, 8.191099868251446680E-34, 1.000000000000000000 ) ) ;
#3835 = CARTESIAN_POINT ( 'NONE',  ( -1.693770420379220099, -13.89774397934251837, 37.86118342676929416 ) ) ;
#3836 = ADVANCED_FACE ( 'NONE', ( #5258 ), #3094, .F. ) ;
#3837 = ORIENTED_EDGE ( 'NONE', *, *, #290, .F. ) ;
#3838 = CARTESIAN_POINT ( 'NONE',  ( -12.22833218042443271, 7.529642458189139909, 7.781673716087849968 ) ) ;
#3839 = VERTEX_POINT ( 'NONE', #2883 ) ;
#3840 = CARTESIAN_POINT ( 'NONE',  ( -7.806708723663831506, -7.806708723663902560, 5.250000000000008882 ) ) ;
#3841 = CARTESIAN_POINT ( 'NONE',  ( -5.284464991282755264, 15.10213328493384743, 30.42857142857143060 ) ) ;
#3842 = CARTESIAN_POINT ( 'NONE',  ( -156.0000000000000284, -16.00000000000000711, 0.000000000000000000 ) ) ;
#3843 = CARTESIAN_POINT ( 'NONE',  ( -14.28433602490915000, 1.478298951650542481, 31.35310228751642470 ) ) ;
#3844 = CARTESIAN_POINT ( 'NONE',  ( -1.595456901104623348, 10.37818827243067155, 8.301137918078554279 ) ) ;
#3845 = CARTESIAN_POINT ( 'NONE',  ( 9.375578539472099848, -1.533232399699987702, 3.201137918078536426 ) ) ;
#3846 = DIRECTION ( 'NONE',  ( 0.000000000000000000, 1.000000000000000000, 0.000000000000000000 ) ) ;
#3847 = CARTESIAN_POINT ( 'NONE',  ( -9.809645194534070356, 9.989344678689256796, 10.00404056962643651 ) ) ;
#3848 = CARTESIAN_POINT ( 'NONE',  ( -7.639999817571787588, 12.15899005565156266, 48.21428571428570820 ) ) ;
#3849 = EDGE_LOOP ( 'NONE', ( #8264, #8474, #738, #9255 ) ) ;
#3850 = CARTESIAN_POINT ( 'NONE',  ( -8.841785722321695573, 13.82664651025757152, 14.21024514465927702 ) ) ;
#3851 = CARTESIAN_POINT ( 'NONE',  ( -160.0000000000000284, 14.99999999999999289, 0.000000000000000000 ) ) ;
#3852 = CARTESIAN_POINT ( 'NONE',  ( 13.89598863503046111, -8.731428362939032795, 38.78571428571429180 ) ) ;
#3853 = FACE_OUTER_BOUND ( 'NONE', #2322, .T. ) ;
#3854 = DIRECTION ( 'NONE',  ( -1.000000000000000000, 1.842239752758738928E-31, -1.780435181894459419E-32 ) ) ;
#3855 = CARTESIAN_POINT ( 'NONE',  ( -4.534861676072319270, 8.900167166472122915, 9.150000000000003908 ) ) ;
#3856 = CARTESIAN_POINT ( 'NONE',  ( -4.534861676072319270, 8.900167166472121139, 0.1499999999999952482 ) ) ;
#3857 = FACE_OUTER_BOUND ( 'NONE', #6839, .T. ) ;
#3858 = CARTESIAN_POINT ( 'NONE',  ( -11.60466159355861926, -11.60466159355875249, 40.50000000000000711 ) ) ;
#3859 = B_SPLINE_CURVE_WITH_KNOTS ( 'NONE', 3,
 ( #3330, #5741, #2644, #8910, #1003, #5795, #6511, #9645, #4929, #7402, #326, #225, #277, #8969, #955, #2551, #1731, #1109, #8127, #170, #4980, #5030, #6466, #2499, #4105, #120, #7354, #1882 ),
 .UNSPECIFIED., .F., .F.,
 ( 4, 2, 2, 2, 2, 2, 2, 2, 2, 2, 2, 2, 2, 4 ),
 ( 0.006730547602530746569, 0.007571661104541401940, 0.007992217855546712713, 0.008412774606552025219, 0.008833331357557337726, 0.009253888108562648498, 0.009674444859567959271, 0.01009500161057327178, 0.01051555836157858255, 0.01093611511258389332, 0.01135667186358920583, 0.01177722861459451487, 0.01261834211660513988, 0.01345945561861576142 ),
 .UNSPECIFIED. ) ;
#3860 = SHAPE_REPRESENTATION_RELATIONSHIP ( 'NONE' , 'NONE' ,  #3478, #8455 ) ;
#3861 = CARTESIAN_POINT ( 'NONE',  ( 5.543385399275644332, 15.44746603149420494, 17.07546914105500591 ) ) ;
#3862 = CARTESIAN_POINT ( 'NONE',  ( -13.89598863503046111, 8.731428362939027465, 23.78571428571429536 ) ) ;
#3863 = CARTESIAN_POINT ( 'NONE',  ( 1.805317605496833622, 15.89926306122265309, 48.73000000000001108 ) ) ;
#3864 = CARTESIAN_POINT ( 'NONE',  ( -1.727091770866549414, -10.90442828429184630, 16.94999999999998863 ) ) ;
#3865 = CARTESIAN_POINT ( 'NONE',  ( -11.31370849898482156, 11.31370849898469544, 48.00000000000000000 ) ) ;
#3866 = CARTESIAN_POINT ( 'NONE',  ( -1.677562661911643938, -10.91227292449344688, 5.948862081921430622 ) ) ;
#3867 = CARTESIAN_POINT ( 'NONE',  ( 13.89598863503046111, -8.731428362939032795, 2.785714285714284255 ) ) ;
#3868 = CARTESIAN_POINT ( 'NONE',  ( 1.791431617652837316, 15.89939535829188877, 0.8571428571428549859 ) ) ;
#3869 = ITEM_DEFINED_TRANSFORMATION ( 'NONE', 'NONE', #6061,  #3995 ) ;
#3870 = CARTESIAN_POINT ( 'NONE',  ( -10.15407889436378852, -10.15407889436390398, 22.50000000000000355 ) ) ;
#3871 = ADVANCED_FACE ( 'NONE', ( #9206, #7705 ), #3877, .F. ) ;
#3872 = CARTESIAN_POINT ( 'NONE',  ( 1.693770420379222319, 13.89774397934251837, 34.86118342676929416 ) ) ;
#3873 = CARTESIAN_POINT ( 'NONE',  ( 9.383039235653818366, -1.486127417882129986, 10.19999999999998685 ) ) ;
#3874 = ORIENTED_EDGE ( 'NONE', *, *, #10088, .T. ) ;
#3875 = CARTESIAN_POINT ( 'NONE',  ( 7.750357176954296712, -12.08964793087877787, 35.21024514465927524 ) ) ;
#3876 = EDGE_LOOP ( 'NONE', ( #540, #5439 ) ) ;
#3877 = PLANE ( 'NONE',  #8542 ) ;
#3878 = CARTESIAN_POINT ( 'NONE',  ( -16.32287076676382398, 1.707986654103809343, 25.35310228751642470 ) ) ;
#3879 = CARTESIAN_POINT ( 'NONE',  ( 8.512513224245308763, 13.54758718765259040, 7.285714285714284699 ) ) ;
#3880 = CARTESIAN_POINT ( 'NONE',  ( -1.533232399700100057, 9.375578539472089190, 13.29886208192143471 ) ) ;
#3881 = CARTESIAN_POINT ( 'NONE',  ( -15.88516839912898071, -1.917699372586004980, 25.13881657323070939 ) ) ;
#3882 = CARTESIAN_POINT ( 'NONE',  ( -1.642561882922479732, 10.37072757624895303, 3.299999999999969624 ) ) ;
#3883 = CARTESIAN_POINT ( 'NONE',  ( -1.642561882922479732, 10.37072757624895303, 3.299999999999969624 ) ) ;
#3884 = DIRECTION ( 'NONE',  ( 1.000000000000000000, 0.000000000000000000, 0.000000000000000000 ) ) ;
#3885 = CARTESIAN_POINT ( 'NONE',  ( -156.0000000000000284, -2.164934898019055569E-14, 0.000000000000000000 ) ) ;
#3886 = ORIENTED_EDGE ( 'NONE', *, *, #3567, .T. ) ;
#3887 = CARTESIAN_POINT ( 'NONE',  ( -1.737328882695368115, 14.25515036105620581, 2.638816573230710727 ) ) ;
#3888 = CARTESIAN_POINT ( 'NONE',  ( 7.806708723663832394, 7.806708723663931870, 3.749999999999997780 ) ) ;
#3889 = DIRECTION ( 'NONE',  ( -2.465190328815661345E-32, -0.4999999999999987232, 0.8660254037844392627 ) ) ;
#3890 = CARTESIAN_POINT ( 'NONE',  ( -1.441234910513241818, -13.92619789766829008, 29.85310228751642470 ) ) ;
#3891 = CARTESIAN_POINT ( 'NONE',  ( -9.377220287598998283, -4.724406229267460233, 7.401137918078573463 ) ) ;
#3892 = CARTESIAN_POINT ( 'NONE',  ( 4.355403765523470305, 8.442910196168369907, 5.601137918078562983 ) ) ;
#3893 = CARTESIAN_POINT ( 'NONE',  ( -168.0000000000000284, -11.00000000000000533, 0.000000000000000000 ) ) ;
#3894 = CARTESIAN_POINT ( 'NONE',  ( 14.25515036105622535, -1.737328882695210241, 0.3611834267692887734 ) ) ;
#3895 = ADVANCED_FACE ( 'NONE', ( #6854 ), #9411, .F. ) ;
#3896 = CARTESIAN_POINT ( 'NONE',  ( 4.623906867372411078, -13.21436662431711717, 45.42857142857143060 ) ) ;
#3897 = ORIENTED_EDGE ( 'NONE', *, *, #9778, .T. ) ;
#3898 = CARTESIAN_POINT ( 'NONE',  ( 8.404922754268618235, 13.61519076058357491, 9.281673716087846415 ) ) ;
#3899 = DIRECTION ( 'NONE',  ( -1.000000000000000000, 0.000000000000000000, 0.000000000000000000 ) ) ;
#3900 = CARTESIAN_POINT ( 'NONE',  ( 8.731428362939190890, -13.89598863503036164, 39.21428571428571530 ) ) ;
#3901 = PLANE ( 'NONE',  #10093 ) ;
#3902 = DIRECTION ( 'NONE',  ( 0.000000000000000000, -6.338944243255235518E-49, 1.000000000000000000 ) ) ;
#3903 = CARTESIAN_POINT ( 'NONE',  ( 9.873755945037075321, 1.513077731353043909, 0.05113791807855379290 ) ) ;
#3904 = CARTESIAN_POINT ( 'NONE',  ( 8.464561979789474222, 4.312909747525755400, 0.9000000000000119016 ) ) ;
#3905 = CYLINDRICAL_SURFACE ( 'NONE', #1005, 20.00000000000000000 ) ;
#3906 = LINE ( 'NONE', #4060, #3462 ) ;
#3907 = CARTESIAN_POINT ( 'NONE',  ( 13.82664651025767100, -8.841785722321541030, 30.78975485534071765 ) ) ;
#3908 = CARTESIAN_POINT ( 'NONE',  ( 13.89598863503046111, -8.731428362939032795, 20.78571428571429180 ) ) ;
#3909 = CARTESIAN_POINT ( 'NONE',  ( -55.00000000000002132, 1.501835218140771437E-15, -12.99999999999999822 ) ) ;
#3910 = CARTESIAN_POINT ( 'NONE',  ( 13.89598863503046111, -8.731428362939032795, 8.785714285714293581 ) ) ;
#3911 = AXIS2_PLACEMENT_3D ( 'NONE', #4877, #66, #274 ) ;
#3912 = CARTESIAN_POINT ( 'NONE',  ( 9.859792900771104485, -4.967534682030588122, 11.34886208192143364 ) ) ;
#3913 = CARTESIAN_POINT ( 'NONE',  ( -11.60466159355861926, -11.60466159355875249, 4.500000000000005329 ) ) ;
#3914 = CARTESIAN_POINT ( 'NONE',  ( -15.49051278174638036, -5.420364854932175902, 10.92857142857142883 ) ) ;
#3915 = CONTEXT_DEPENDENT_SHAPE_REPRESENTATION ( #8229, #3667 ) ;
#3916 = CARTESIAN_POINT ( 'NONE',  ( 4.623906867372411078, -13.21436662431711717, 45.42857142857143060 ) ) ;
#3917 = CARTESIAN_POINT ( 'NONE',  ( 11.92174236212692229, 7.340858601238088532, 29.71832628391214826 ) ) ;
#3918 = CARTESIAN_POINT ( 'NONE',  ( -7.063212654743467489, -7.063212654743535879, 8.250000000000030198 ) ) ;
#3919 = CIRCLE ( 'NONE', #623, 17.72919999999999874 ) ;
#3920 = CARTESIAN_POINT ( 'NONE',  ( 7.771249796623105333, 7.842167650704658932, 1.748862081921432887 ) ) ;
#3921 = EDGE_LOOP ( 'NONE', ( #2431, #1067, #5523, #7212 ) ) ;
#3922 = CARTESIAN_POINT ( 'NONE',  ( 13.21436662431716869, -4.623906867372263640, 8.571428571428569398 ) ) ;
#3923 = VERTEX_POINT ( 'NONE', #1500 ) ;
#3924 = DIRECTION ( 'NONE',  ( 1.000000000000000000, 0.000000000000000000, 0.000000000000000000 ) ) ;
#3925 = CARTESIAN_POINT ( 'NONE',  ( 13.47998361472151529, 8.620103694222146729, 21.71024514465928235 ) ) ;
#3926 = COLOUR_RGB ( '', 0.40784314, 0.44705882, 0.49803922) ;
#3927 = CARTESIAN_POINT ( 'NONE',  ( 15.49051278174637858, 5.420364854932174126, 1.928571428571430380 ) ) ;
#3928 = CARTESIAN_POINT ( 'NONE',  ( 8.841785722321695573, -13.82664651025757152, 17.21024514465927879 ) ) ;
#3929 = CARTESIAN_POINT ( 'NONE',  ( -88.00000000000002842, 0.000000000000000000, 0.000000000000000000 ) ) ;
#3930 = CARTESIAN_POINT ( 'NONE',  ( 10.37072757624895836, -1.642561882922355609, 4.199999999999981526 ) ) ;
#3931 = DIRECTION ( 'NONE',  ( 0.000000000000000000, 0.000000000000000000, 1.000000000000000000 ) ) ;
#3932 = EDGE_CURVE ( 'NONE', #8337, #7745, #8041, .T. ) ;
#3933 = ADVANCED_FACE ( 'NONE', ( #626, #5370 ), #8634, .F. ) ;
#3934 = CARTESIAN_POINT ( 'NONE',  ( -5.420364854931999155, -15.49051278174644253, 34.07142857142859071 ) ) ;
#3935 = ORIENTED_EDGE ( 'NONE', *, *, #10187, .F. ) ;
#3936 = CARTESIAN_POINT ( 'NONE',  ( 16.32287076676382043, -1.707986654103810897, 46.35310228751641404 ) ) ;
#3937 = CARTESIAN_POINT ( 'NONE',  ( -10.90442828429184274, -1.727091770866655107, 2.550000000000035794 ) ) ;
#3938 = FACE_OUTER_BOUND ( 'NONE', #4483, .T. ) ;
#3939 = CARTESIAN_POINT ( 'NONE',  ( -7.340858601237953529, -11.92174236212700222, 24.28167371608785530 ) ) ;
#3940 = CARTESIAN_POINT ( 'NONE',  ( 4.967534682030706250, -9.859792900771036983, 0.6511379180785785703 ) ) ;
#3941 = CARTESIAN_POINT ( 'NONE',  ( -1.595456901104623348, 10.37818827243067155, -0.6988620819214501623 ) ) ;
#3942 = DIRECTION ( 'NONE',  ( -1.000000000000000000, 0.000000000000000000, 0.000000000000000000 ) ) ;
#3943 = CARTESIAN_POINT ( 'NONE',  ( 1.478298951650704351, -14.28433602490913579, 1.646897712483578857 ) ) ;
#3944 = CARTESIAN_POINT ( 'NONE',  ( 13.92619789766827587, 1.441234910513398582, 18.14689771248357530 ) ) ;
#3945 = ORIENTED_EDGE ( 'NONE', *, *, #9868, .T. ) ;
#3946 = CARTESIAN_POINT ( 'NONE',  ( -8.404922754268618235, -13.61519076058357491, 12.28167371608784997 ) ) ;
#3947 = CARTESIAN_POINT ( 'NONE',  ( 2.000000000000001776, 1.773042676681366281, 0.000000000000000000 ) ) ;
#3948 = CARTESIAN_POINT ( 'NONE',  ( -15.89939535829186923, -1.791431617653016062, 47.14285714285714590 ) ) ;
#3949 = DIRECTION ( 'NONE',  ( 1.000000000000000000, 0.000000000000000000, 0.000000000000000000 ) ) ;
#3950 = CARTESIAN_POINT ( 'NONE',  ( 8.464561979789474222, 4.312909747525755400, 12.90000000000002345 ) ) ;
#3951 = CARTESIAN_POINT ( 'NONE',  ( -6.717514421272238856, 6.717514421272176683, 3.000000000000002665 ) ) ;
#3952 = ADVANCED_FACE ( 'NONE', ( #4653 ), #6965, .T. ) ;
#3953 = CYLINDRICAL_SURFACE ( 'NONE', #6266, 18.00000000000000355 ) ;
#3954 = CARTESIAN_POINT ( 'NONE',  ( -1.707986654103994528, 16.32287076676380266, 28.64689771248357886 ) ) ;
#3955 = CARTESIAN_POINT ( 'NONE',  ( 9.865911304835478290, 1.562606840307948941, 4.049999999999988276 ) ) ;
#3956 = SHAPE_REPRESENTATION ( 'main spring', ( #3995 ), #5075 ) ;
#3957 = CARTESIAN_POINT ( 'NONE',  ( 15.06016580658428694, -5.404401153735007846, 30.57546914105500946 ) ) ;
#3958 = ORIENTED_EDGE ( 'NONE', *, *, #5485, .F. ) ;
#3959 = ADVANCED_FACE ( 'NONE', ( #1346 ), #6184, .F. ) ;
#3960 = VECTOR ( 'NONE', #9493, 1000.000000000000000 ) ;
#3961 = CARTESIAN_POINT ( 'NONE',  ( 13.54758718765249803, 8.512513224245457977, 13.71428571428571352 ) ) ;
#3962 = CARTESIAN_POINT ( 'NONE',  ( -7.133621909761823559E-16, 15.00000000000000000, 0.000000000000000000 ) ) ;
#3963 = ORIENTED_EDGE ( 'NONE', *, *, #9284, .T. ) ;
#3964 = FACE_OUTER_BOUND ( 'NONE', #6307, .T. ) ;
#3965 = CARTESIAN_POINT ( 'NONE',  ( -160.0000000000000284, -7.609196703745946707E-15, 0.000000000000000000 ) ) ;
#3966 =( NAMED_UNIT ( * ) SI_UNIT ( $, .STERADIAN. ) SOLID_ANGLE_UNIT ( ) );
#3967 = CARTESIAN_POINT ( 'NONE',  ( 4.724406229267374968, 9.377220287599060455, 10.59886208192144075 ) ) ;
#3968 = CARTESIAN_POINT ( 'NONE',  ( 13.92619789766827587, 1.441234910513398582, 42.14689771248358596 ) ) ;
#3969 = AXIS2_PLACEMENT_3D ( 'NONE', #4154, #8817, #4880 ) ;
#3970 = CARTESIAN_POINT ( 'NONE',  ( -13.54758718765249625, -8.512513224245459753, 16.71428571428571530 ) ) ;
#3971 = CIRCLE ( 'NONE', #9752, 18.00000000000000355 ) ;
#3972 = CARTESIAN_POINT ( 'NONE',  ( 11.85413878919593422, 7.448449071214774619, 37.71428571428571530 ) ) ;
#3973 = CARTESIAN_POINT ( 'NONE',  ( -8.900167166472160218, 4.534861676072232228, 8.850000000000010303 ) ) ;
#3974 = CARTESIAN_POINT ( 'NONE',  ( -1.689666864740335228, 10.36326688006723273, 1.298862081921425604 ) ) ;
#3975 = ORIENTED_EDGE ( 'NONE', *, *, #2410, .T. ) ;
#3976 = CARTESIAN_POINT ( 'NONE',  ( 9.809645194533960222, 9.989344678689363377, 51.49595943037355994 ) ) ;
#3977 = AXIS2_PLACEMENT_3D ( 'NONE', #1118, #5704, #7363 ) ;
#3978 = ORIENTED_EDGE ( 'NONE', *, *, #8156, .F. ) ;
#3979 = DIRECTION ( 'NONE',  ( -1.000000000000000000, 1.842239752758738928E-31, 1.840628461782073167E-32 ) ) ;
#3980 = CARTESIAN_POINT ( 'NONE',  ( -15.14410076328353227, 5.164528828830164287, 31.56738800180213644 ) ) ;
#3981 = AXIS2_PLACEMENT_3D ( 'NONE', #1353, #633, #7600 ) ;
#3982 = CARTESIAN_POINT ( 'NONE',  ( -15.49051278174637858, -5.420364854932175014, 22.92857142857143060 ) ) ;
#3983 = CARTESIAN_POINT ( 'NONE',  ( -1.967016585148659846, 16.29368510291087091, 20.63881657323070939 ) ) ;
#3984 = CARTESIAN_POINT ( 'NONE',  ( 0.000000000000000000, 0.000000000000000000, 0.000000000000000000 ) ) ;
#3985 = CARTESIAN_POINT ( 'NONE',  ( -1.727091770866549414, -10.90442828429185695, 4.950000000000017053 ) ) ;
#3986 = PLANE ( 'NONE',  #7782 ) ;
#3987 = CIRCLE ( 'NONE', #4973, 15.00000000000000178 ) ;
#3988 = AXIS2_PLACEMENT_3D ( 'NONE', #5116, #2185, #2943 ) ;
#3989 = ORIENTED_EDGE ( 'NONE', *, *, #4905, .T. ) ;
#3990 = CARTESIAN_POINT ( 'NONE',  ( 9.989344678689365153, -9.809645194533958446, 10.99595943037356882 ) ) ;
#3991 = ORIENTED_EDGE ( 'NONE', *, *, #2679, .T. ) ;
#3992 = CARTESIAN_POINT ( 'NONE',  ( -10.37072757624895836, 1.642561882922381145, 8.700000000000041922 ) ) ;
#3993 = ADVANCED_FACE ( 'NONE', ( #2936 ), #6026, .T. ) ;
#3994 = FACE_OUTER_BOUND ( 'NONE', #10023, .T. ) ;
#3995 = AXIS2_PLACEMENT_3D ( 'NONE', #245, #8930, #7419 ) ;
#3996 = CARTESIAN_POINT ( 'NONE',  ( -12.22833218042443271, 7.529642458189139909, 25.78167371608785530 ) ) ;
#3997 = CARTESIAN_POINT ( 'NONE',  ( -4.967534682030703586, 9.859792900771061852, 8.151137918078559252 ) ) ;
#3998 = CARTESIAN_POINT ( 'NONE',  ( -9.375578539472099848, 1.533232399700011683, 10.70113791807854220 ) ) ;
#3999 = CYLINDRICAL_SURFACE ( 'NONE', #4635, 13.00000000000000000 ) ;
#4000 = CARTESIAN_POINT ( 'NONE',  ( 13.92619789766827587, 1.441234910513398582, 12.14689771248358063 ) ) ;
#4001 = CARTESIAN_POINT ( 'NONE',  ( -12.08964793087886314, 7.750357176954159932, 9.789754855340722983 ) ) ;
#4002 = ORIENTED_EDGE ( 'NONE', *, *, #3738, .F. ) ;
#4003 = CIRCLE ( 'NONE', #3005, 15.44569104238500046 ) ;
#4004 = CARTESIAN_POINT ( 'NONE',  ( -158.0000000000000284, -6.938893903907228378E-15, 0.000000000000000000 ) ) ;
#4005 = CARTESIAN_POINT ( 'NONE',  ( -5.404401153735176599, 15.06016580658422477, 2.424530858944988321 ) ) ;
#4006 = FACE_OUTER_BOUND ( 'NONE', #10045, .T. ) ;
#4007 = CARTESIAN_POINT ( 'NONE',  ( 4.534861676072320158, -8.900167166472098046, 16.64999999999999858 ) ) ;
#4008 = CARTESIAN_POINT ( 'NONE',  ( -4.312909747525649706, -8.464561979789507973, 5.099999999999993427 ) ) ;
#4009 = DIRECTION ( 'NONE',  ( -4.755747939841215952E-17, 1.000000000000000000, 0.000000000000000000 ) ) ;
#4010 = CARTESIAN_POINT ( 'NONE',  ( -5.164528828830334817, 15.14410076328347543, 28.43261199819786356 ) ) ;
#4011 = CARTESIAN_POINT ( 'NONE',  ( -68.00000000000002842, 0.000000000000000000, 0.000000000000000000 ) ) ;
#4012 = CARTESIAN_POINT ( 'NONE',  ( 8.621071003556677326, -13.96533075980314287, 37.21832628391215536 ) ) ;
#4013 = ORIENTED_EDGE ( 'NONE', *, *, #10208, .T. ) ;
#4014 = CARTESIAN_POINT ( 'NONE',  ( -5.420364854931999155, -15.49051278174644253, 34.07142857142859071 ) ) ;
#4015 = CARTESIAN_POINT ( 'NONE',  ( 5.986002070941135678, -13.58603705635637304, 0.000000000000000000 ) ) ;
#4016 = AXIS2_PLACEMENT_3D ( 'NONE', #1302, #9216, #380 ) ;
#4017 = CARTESIAN_POINT ( 'NONE',  ( 2.000000000000001776, -0.8865213383406761460, 1.535499999999911935 ) ) ;
#4018 = DIRECTION ( 'NONE',  ( -1.000000000000000000, -0.000000000000000000, -0.000000000000000000 ) ) ;
#4019 = CARTESIAN_POINT ( 'NONE',  ( 7.771249796623105333, 7.842167650704654491, 13.74886208192144643 ) ) ;
#4020 = CIRCLE ( 'NONE', #9612, 2.000000000000001332 ) ;
#4021 = PRODUCT_DEFINITION_CONTEXT ( 'detailed design', #3283, 'design' ) ;
#4022 = CARTESIAN_POINT ( 'NONE',  ( 9.859792900771104485, -4.967534682030585458, 14.34886208192142831 ) ) ;
#4023 = CARTESIAN_POINT ( 'NONE',  ( 1.917699372585825790, 15.88516839912900203, -1.138816573230706286 ) ) ;
#4024 = CARTESIAN_POINT ( 'NONE',  ( -15.49051278174638036, -5.420364854932175902, 16.92857142857143771 ) ) ;
#4025 = ITEM_DEFINED_TRANSFORMATION ( 'NONE', 'NONE', #2288,  #3995 ) ;
#4026 = CARTESIAN_POINT ( 'NONE',  ( -12.15899005565164792, 7.639999817571650809, 41.78571428571429180 ) ) ;
#4027 = CARTESIAN_POINT ( 'NONE',  ( -12.08964793087886314, 7.750357176954159932, 45.78975485534073897 ) ) ;
#4028 = CARTESIAN_POINT ( 'NONE',  ( -13.21436662431716869, 4.623906867372262752, 5.571428571428574728 ) ) ;
#4029 = CARTESIAN_POINT ( 'NONE',  ( 7.063212654743468377, 7.063212654743558083, 6.749999999999960920 ) ) ;
#4030 = CARTESIAN_POINT ( 'NONE',  ( -4.766900247265192014, -9.355568503977876205, 17.10000000000000497 ) ) ;
#4031 = VERTEX_POINT ( 'NONE', #3717 ) ;
#4032 = CARTESIAN_POINT ( 'NONE',  ( -10.15407889436378852, -10.15407889436390576, 4.500000000000005329 ) ) ;
#4033 = ORIENTED_EDGE ( 'NONE', *, *, #6419, .F. ) ;
#4034 = DIRECTION ( 'NONE',  ( 0.000000000000000000, 0.000000000000000000, 1.000000000000000000 ) ) ;
#4035 = CARTESIAN_POINT ( 'NONE',  ( -1.791431617652833763, -15.89939535829188877, 21.85714285714286120 ) ) ;
#4036 = CARTESIAN_POINT ( 'NONE',  ( -15.44746603149413922, -5.543385399275820191, 42.92453085894499054 ) ) ;
#4037 = CARTESIAN_POINT ( 'NONE',  ( -2.000000000000000888, -16.99999999999997868, 2.081899558550498307E-15 ) ) ;
#4038 = CARTESIAN_POINT ( 'NONE',  ( -10.90442828429183919, -1.727091770866655329, 5.549999999999999822 ) ) ;
#4039 = CARTESIAN_POINT ( 'NONE',  ( 0.000000000000000000, 1.221245327087672352E-14, 68.00000000000000000 ) ) ;
#4040 = ORIENTED_EDGE ( 'NONE', *, *, #3485, .F. ) ;
#4041 = CARTESIAN_POINT ( 'NONE',  ( -12.22833218042443271, 7.529642458189139909, 13.78167371608785174 ) ) ;
#4042 = CARTESIAN_POINT ( 'NONE',  ( -10.37072757624895836, 1.642561882922380034, 11.69999999999998863 ) ) ;
#4043 = CARTESIAN_POINT ( 'NONE',  ( 1.837501619626330074, -16.30827793483733501, 15.64285714285714235 ) ) ;
#4044 = CARTESIAN_POINT ( 'NONE',  ( -158.0000000000000284, -6.938893903907228378E-15, 0.000000000000000000 ) ) ;
#4045 = CARTESIAN_POINT ( 'NONE',  ( 10.91227292449344155, 1.677562661911773167, 6.051137918078538291 ) ) ;
#4046 = CARTESIAN_POINT ( 'NONE',  ( 1.612135949262739398, 9.858066664633906129, 14.45113791807853509 ) ) ;
#4047 = DIRECTION ( 'NONE',  ( -0.000000000000000000, -0.000000000000000000, 1.000000000000000000 ) ) ;
#4048 = CARTESIAN_POINT ( 'NONE',  ( -13.17239914596754424, 4.743843029824683200, 3.575469141055005462 ) ) ;
#4049 = CARTESIAN_POINT ( 'NONE',  ( -10.24623928997352351, -10.06191849875416899, 14.50404056962643651 ) ) ;
#4050 = EDGE_LOOP ( 'NONE', ( #1129, #5484 ) ) ;
#4051 = DIRECTION ( 'NONE',  ( 1.000000000000000000, 0.000000000000000000, 0.000000000000000000 ) ) ;
#4052 = CARTESIAN_POINT ( 'NONE',  ( 15.10213328493390783, -5.284464991282587398, 44.57142857142857650 ) ) ;
#4053 = CARTESIAN_POINT ( 'NONE',  ( -164.2691053559693728, -1.483232571104735609, 12.91517534017533109 ) ) ;
#4054 = DIRECTION ( 'NONE',  ( -1.000000000000000000, 0.000000000000000000, -0.000000000000000000 ) ) ;
#4055 = CARTESIAN_POINT ( 'NONE',  ( -4.534861676072319270, 8.900167166472121139, 15.14999999999998259 ) ) ;
#4056 = CARTESIAN_POINT ( 'NONE',  ( -8.900167166472156666, 4.534861676072234893, 5.849999999999989875 ) ) ;
#4057 = ADVANCED_FACE ( 'NONE', ( #6078, #9256 ), #2178, .F. ) ;
#4058 = CARTESIAN_POINT ( 'NONE',  ( -166.0823889414796497, 1.878652528652014819, 12.86399816373932126 ) ) ;
#4059 = CARTESIAN_POINT ( 'NONE',  ( 15.91362231745475597, 1.665163862720026255, 30.14689771248358241 ) ) ;
#4060 = CARTESIAN_POINT ( 'NONE',  ( -108.0000000000000284, 0.000000000000000000, 16.00000000000000000 ) ) ;
#4061 = CARTESIAN_POINT ( 'NONE',  ( -8.621071003556675549, 13.96533075980314642, 34.21832628391215536 ) ) ;
#4062 = ORIENTED_EDGE ( 'NONE', *, *, #8698, .T. ) ;
#4063 = CARTESIAN_POINT ( 'NONE',  ( 15.89939535829187278, 1.791431617653015174, 32.14285714285714590 ) ) ;
#4064 = CARTESIAN_POINT ( 'NONE',  ( 3.896594582693065245, 14.56547797550490309, 3.589645083274735104E-17 ) ) ;
#4065 = ORIENTED_EDGE ( 'NONE', *, *, #10020, .T. ) ;
#4066 = DIRECTION ( 'NONE',  ( 1.000000000000000000, 0.000000000000000000, 0.000000000000000000 ) ) ;
#4067 = PRESENTATION_STYLE_ASSIGNMENT (( #2511 ) ) ;
#4068 = CARTESIAN_POINT ( 'NONE',  ( -1.689666864740335228, 10.36326688006723451, 16.29886208192143471 ) ) ;
#4069 = CARTESIAN_POINT ( 'NONE',  ( -15.91362231745475597, -1.665163862720028254, 3.146897712483577969 ) ) ;
#4070 = CARTESIAN_POINT ( 'NONE',  ( 1.837501619626330074, -16.30827793483733501, 21.64285714285714590 ) ) ;
#4071 = CARTESIAN_POINT ( 'NONE',  ( 13.55419868402807992, 4.742819248065649695, 37.92857142857143060 ) ) ;
#4072 = CARTESIAN_POINT ( 'NONE',  ( 1.693770420379222319, 13.89774397934251837, 40.86118342676929416 ) ) ;
#4073 = CARTESIAN_POINT ( 'NONE',  ( 7.448449071214646722, 11.85413878919601594, 7.285714285714284699 ) ) ;
#4074 = DIRECTION ( 'NONE',  ( 0.000000000000000000, -6.338944243255235518E-49, 1.000000000000000000 ) ) ;
#4075 = CARTESIAN_POINT ( 'NONE',  ( -7.458344646081709328, 7.390897758835805575, 6.998862081921422451 ) ) ;
#4076 = CARTESIAN_POINT ( 'NONE',  ( 10.15407889436379030, 10.15407889436390576, 7.500000000000005329 ) ) ;
#4077 = CARTESIAN_POINT ( 'NONE',  ( 56.99999999999997158, 0.000000000000000000, 0.000000000000000000 ) ) ;
#4078 = CARTESIAN_POINT ( 'NONE',  ( -5.420364854931998266, -15.49051278174643898, 16.07142857142857650 ) ) ;
#4079 = CARTESIAN_POINT ( 'NONE',  ( 13.47998361472151529, 8.620103694222146729, 39.71024514465927524 ) ) ;
#4080 = CARTESIAN_POINT ( 'NONE',  ( 7.806708723663831506, 7.806708723663930982, 12.75000000000000533 ) ) ;
#4081 = CARTESIAN_POINT ( 'NONE',  ( 7.806708723663831506, 7.806708723663930982, 0.7499999999999762412 ) ) ;
#4082 = ADVANCED_FACE ( 'NONE', ( #7899 ), #775, .F. ) ;
#4083 = CARTESIAN_POINT ( 'NONE',  ( 2.000000000000001776, -0.8865213383406761460, 1.535499999999911935 ) ) ;
#4084 = AXIS2_PLACEMENT_3D ( 'NONE', #5623, #7129, #45 ) ;
#4085 = VERTEX_POINT ( 'NONE', #8002 ) ;
#4086 = CARTESIAN_POINT ( 'NONE',  ( -9.989344678689363377, 9.809645194533960222, 13.99595943037356527 ) ) ;
#4087 = CARTESIAN_POINT ( 'NONE',  ( -7.424621202458789426, 7.424621202458724589, 18.00000000000001421 ) ) ;
#4088 = CARTESIAN_POINT ( 'NONE',  ( -11.31370849898482156, 11.31370849898469544, 11.99999999999999645 ) ) ;
#4089 = CARTESIAN_POINT ( 'NONE',  ( -165.5312037683856943, 1.565894570282060583, 12.90541399993123228 ) ) ;
#4090 = CARTESIAN_POINT ( 'NONE',  ( 13.54758718765249803, 8.512513224245457977, 37.71428571428571530 ) ) ;
#4091 = CARTESIAN_POINT ( 'NONE',  ( -11.78653521626494793, -7.556039541191465148, 36.71024514465928235 ) ) ;
#4092 = CARTESIAN_POINT ( 'NONE',  ( -9.814260835641038128, 5.056896391392218248, 16.85113791807854611 ) ) ;
#4093 = CARTESIAN_POINT ( 'NONE',  ( -4.355403765523468529, -8.442910196168346815, 16.10113791807856742 ) ) ;
#4094 = EDGE_CURVE ( 'NONE', #8205, #2970, #4412, .T. ) ;
#4095 = STYLED_ITEM ( 'NONE', ( #7763 ), #4260 ) ;
#4096 = CARTESIAN_POINT ( 'NONE',  ( -158.0000000000000284, 15.99999999999998934, 1.959434878635764737E-15 ) ) ;
#4097 = CARTESIAN_POINT ( 'NONE',  ( -13.59724543428031573, -4.619798703722008959, 14.93261199819787066 ) ) ;
#4098 = ADVANCED_FACE ( 'NONE', ( #3356 ), #2594, .F. ) ;
#4099 = CARTESIAN_POINT ( 'NONE',  ( 1.478298951650704351, -14.28433602490913579, 7.646897712483577969 ) ) ;
#4100 = ORIENTED_EDGE ( 'NONE', *, *, #9010, .T. ) ;
#4101 = DIRECTION ( 'NONE',  ( 0.000000000000000000, 8.191099868251446680E-34, 1.000000000000000000 ) ) ;
#4102 = CARTESIAN_POINT ( 'NONE',  ( -13.47998361472151174, -8.620103694222146729, 12.71024514465927879 ) ) ;
#4103 = PRODUCT_DEFINITION_FORMATION_WITH_SPECIFIED_SOURCE ( 'ANY', '', #7568, .NOT_KNOWN. ) ;
#4104 = CARTESIAN_POINT ( 'NONE',  ( -108.0000000000000284, 0.000000000000000000, 8.500000000000000000 ) ) ;
#4105 = CARTESIAN_POINT ( 'NONE',  ( -166.8777055324365790, -1.084022349717994604, 14.96301859724961147 ) ) ;
#4106 = CARTESIAN_POINT ( 'NONE',  ( 1.562606840307832368, 9.865911304835510265, 12.44999999999995666 ) ) ;
#4107 = CARTESIAN_POINT ( 'NONE',  ( -8.900167166472156666, 4.534861676072231340, 2.849999999999968114 ) ) ;
#4108 = CARTESIAN_POINT ( 'NONE',  ( 0.000000000000000000, 0.000000000000000000, 0.000000000000000000 ) ) ;
#4109 = CARTESIAN_POINT ( 'NONE',  ( 1.917699372585825790, 15.88516839912900203, 22.86118342676929061 ) ) ;
#4110 = DIRECTION ( 'NONE',  ( 0.000000000000000000, 0.000000000000000000, 1.000000000000000000 ) ) ;
#4111 = CARTESIAN_POINT ( 'NONE',  ( 5.164528828830335705, -15.14410076328347543, 31.43261199819787421 ) ) ;
#4112 = VERTEX_POINT ( 'NONE', #6491 ) ;
#4113 = CARTESIAN_POINT ( 'NONE',  ( 13.54758718765249803, 8.512513224245457977, 37.71428571428571530 ) ) ;
#4114 = CARTESIAN_POINT ( 'NONE',  ( -108.0000000000000284, 1.040949779275250140E-15, -8.500000000000000000 ) ) ;
#4115 = CARTESIAN_POINT ( 'NONE',  ( 16.30827793483735633, -1.837501619626142890, 8.357142857142855874 ) ) ;
#4116 = CARTESIAN_POINT ( 'NONE',  ( 17.72919999999999874, -4.025229594467075325E-49, -1.270000000000007123 ) ) ;
#4117 = CARTESIAN_POINT ( 'NONE',  ( 1.513077731352925115, 9.873755945037103743, 7.448862081921427070 ) ) ;
#4118 = CARTESIAN_POINT ( 'NONE',  ( 7.458344646081711105, -7.390897758835778930, 17.49886208192142689 ) ) ;
#4119 = UNCERTAINTY_MEASURE_WITH_UNIT (LENGTH_MEASURE( 1.000000000000000082E-05 ), #8397, 'distance_accuracy_value', 'NONE');
#4120 = CARTESIAN_POINT ( 'NONE',  ( 13.59724543428031573, 4.619798703722006294, 41.93261199819787066 ) ) ;
#4121 = CARTESIAN_POINT ( 'NONE',  ( -5.420364854931999155, -15.49051278174644253, 10.07142857142856940 ) ) ;
#4122 = CARTESIAN_POINT ( 'NONE',  ( 4.865839792409144771, 13.51115193377589740, 41.07546914105501656 ) ) ;
#4123 = CARTESIAN_POINT ( 'NONE',  ( 13.55419868402807992, 4.742819248065648807, 7.928571428571430602 ) ) ;
#4124 = CARTESIAN_POINT ( 'NONE',  ( 9.865911304835478290, 1.562606840307950273, 16.04999999999995808 ) ) ;
#4125 = CARTESIAN_POINT ( 'NONE',  ( -10.37818827243067688, 1.595456901104525205, 3.698862081921452827 ) ) ;
#4126 = ORIENTED_EDGE ( 'NONE', *, *, #2251, .F. ) ;
#4127 = CARTESIAN_POINT ( 'NONE',  ( -4.623906867372410190, 13.21436662431711895, 0.4285714285714309346 ) ) ;
#4128 = ORIENTED_EDGE ( 'NONE', *, *, #9269, .F. ) ;
#4129 = DIRECTION ( 'NONE',  ( -1.000000000000000000, 0.000000000000000000, 0.000000000000000000 ) ) ;
#4130 = CARTESIAN_POINT ( 'NONE',  ( 5.284464991282756152, -15.10213328493384743, 21.42857142857142705 ) ) ;
#4131 = VECTOR ( 'NONE', #5500, 1000.000000000000114 ) ;
#4132 = CARTESIAN_POINT ( 'NONE',  ( 13.47998361472151529, 8.620103694222146729, 33.71024514465927524 ) ) ;
#4133 = CARTESIAN_POINT ( 'NONE',  ( -10.90442828429183919, -1.727091770866655329, 8.549999999999963407 ) ) ;
#4134 = CARTESIAN_POINT ( 'NONE',  ( 1.642561882922480621, -10.37072757624892638, 16.80000000000003624 ) ) ;
#4135 = DIRECTION ( 'NONE',  ( -1.000000000000000000, 0.000000000000000000, 0.000000000000000000 ) ) ;
#4136 = AXIS2_PLACEMENT_3D ( 'NONE', #7162, #8561, #9398 ) ;
#4137 = AXIS2_PLACEMENT_3D ( 'NONE', #3072, #6216, #8452 ) ;
#4138 = VECTOR ( 'NONE', #7969, 1000.000000000000000 ) ;
#4139 = VERTEX_POINT ( 'NONE', #146 ) ;
#4140 = CARTESIAN_POINT ( 'NONE',  ( 10.90442828429184274, 1.727091770866679310, 13.04999999999999538 ) ) ;
#4141 = DIRECTION ( 'NONE',  ( -0.000000000000000000, -0.000000000000000000, 1.000000000000000000 ) ) ;
#4142 = CARTESIAN_POINT ( 'NONE',  ( 9.377220287599001836, 4.724406229267489543, 17.90113791807857524 ) ) ;
#4143 = CARTESIAN_POINT ( 'NONE',  ( 8.877401133907127928, -4.579542530753017537, 15.35113791807859229 ) ) ;
#4144 = AXIS2_PLACEMENT_3D ( 'NONE', #5292, #8449, #2202 ) ;
#4145 = VECTOR ( 'NONE', #10032, 1000.000000000000000 ) ;
#4146 = CARTESIAN_POINT ( 'NONE',  ( -11.48991645990274257, -11.34085470199651979, -1.270000000000007123 ) ) ;
#4147 = CARTESIAN_POINT ( 'NONE',  ( -1.478298951650703019, 14.28433602490913579, 16.64689771248358596 ) ) ;
#4148 = PRESENTATION_STYLE_ASSIGNMENT (( #3323 ) ) ;
#4149 = CARTESIAN_POINT ( 'NONE',  ( 9.809645194534072132, -9.989344678689256796, 7.004040569626434731 ) ) ;
#4150 = VERTEX_POINT ( 'NONE', #7227 ) ;
#4151 = DIRECTION ( 'NONE',  ( -6.162975822039153635E-32, -0.5000000000000011102, -0.8660254037844379305 ) ) ;
#4152 = CARTESIAN_POINT ( 'NONE',  ( 11.51250119794888249, 11.69682198916847682, 15.49595943037356882 ) ) ;
#4153 = DIRECTION ( 'NONE',  ( 0.000000000000000000, -1.000000000000000000, -1.224646799147353454E-16 ) ) ;
#4154 = CARTESIAN_POINT ( 'NONE',  ( 0.000000000000000000, 4.523427693460793966E-32, 0.000000000000000000 ) ) ;
#4155 = CARTESIAN_POINT ( 'NONE',  ( 7.098671581784200768, 7.027753727702831021, 5.751137918078548239 ) ) ;
#4156 = CARTESIAN_POINT ( 'NONE',  ( -4.312909747525649706, -8.464561979789507973, 2.099999999999990763 ) ) ;
#4157 = CARTESIAN_POINT ( 'NONE',  ( -162.8640792231055912, 0.2831181362186585004, 12.99765045411212938 ) ) ;
#4158 = CARTESIAN_POINT ( 'NONE',  ( -5.164528828830334817, 15.14410076328347543, 34.43261199819786356 ) ) ;
#4159 = CLOSED_SHELL ( 'NONE', ( #867, #2453, #9601, #903, #8311, #4969, #1495, #8034, #7277, #3993, #5127, #4712, #4082, #3080, #2847, #5656, #5169, #5270, #3783 ) ) ;
#4160 = CARTESIAN_POINT ( 'NONE',  ( 10.15407889436379030, 10.15407889436390576, 25.50000000000000711 ) ) ;
#4161 = EDGE_CURVE ( 'NONE', #4954, #8895, #3919, .T. ) ;
#4162 = CARTESIAN_POINT ( 'NONE',  ( 15.53355953199861794, 5.297344310588528060, 41.93261199819787066 ) ) ;
#4163 = AXIS2_PLACEMENT_3D ( 'NONE', #4181, #2807, #4955 ) ;
#4164 = VERTEX_POINT ( 'NONE', #1801 ) ;
#4165 = CARTESIAN_POINT ( 'NONE',  ( 11.60466159355862104, 11.60466159355875071, 37.50000000000002842 ) ) ;
#4166 = LINE ( 'NONE', #4114, #4962 ) ;
#4167 = CARTESIAN_POINT ( 'NONE',  ( -5.284464991282755264, 15.10213328493384743, 12.42857142857142705 ) ) ;
#4168 = DIRECTION ( 'NONE',  ( 0.000000000000000000, 0.000000000000000000, 1.000000000000000000 ) ) ;
#4169 = CARTESIAN_POINT ( 'NONE',  ( 9.865911304835474738, 1.562606840307950051, 1.049999999999966738 ) ) ;
#4170 = CARTESIAN_POINT ( 'NONE',  ( 10.37818827243067510, -1.595456901104499448, 14.19886208192146171 ) ) ;
#4171 = CARTESIAN_POINT ( 'NONE',  ( -4.503970704919988854, 13.25633410266674517, 40.43261199819787066 ) ) ;
#4172 = CARTESIAN_POINT ( 'NONE',  ( 8.731428362939190890, -13.89598863503036164, 33.21428571428571530 ) ) ;
#4173 = CARTESIAN_POINT ( 'NONE',  ( 13.92619789766827587, 1.441234910513398582, 42.14689771248358596 ) ) ;
#4174 = AXIS2_PLACEMENT_3D ( 'NONE', #5322, #2938, #7808 ) ;
#4175 = CARTESIAN_POINT ( 'NONE',  ( -1.567502665446231180, -13.91197093850540334, 15.85714285714286120 ) ) ;
#4176 = CARTESIAN_POINT ( 'NONE',  ( 9.383039235653818366, -1.486127417882130208, 19.19999999999999574 ) ) ;
#4177 = CARTESIAN_POINT ( 'NONE',  ( -10.37818827243067688, 1.595456901104524761, 6.698862081921455491 ) ) ;
#4178 = ORIENTED_EDGE ( 'NONE', *, *, #4094, .T. ) ;
#4179 = CARTESIAN_POINT ( 'NONE',  ( 1.607813917173038121, -14.26974319298267346, 21.64285714285714590 ) ) ;
#4180 = ORIENTED_EDGE ( 'NONE', *, *, #6791, .T. ) ;
#4181 = CARTESIAN_POINT ( 'NONE',  ( 0.000000000000000000, 0.000000000000000000, 0.000000000000000000 ) ) ;
#4182 = CARTESIAN_POINT ( 'NONE',  ( -13.89598863503045933, 8.731428362939027465, 11.78571428571428292 ) ) ;
#4183 = CARTESIAN_POINT ( 'NONE',  ( -8.841785722321695573, 13.82664651025757152, 38.21024514465928235 ) ) ;
#4184 = CARTESIAN_POINT ( 'NONE',  ( -9.837026868206066865, 5.012215536711416064, 5.849999999999989875 ) ) ;
#4185 = CARTESIAN_POINT ( 'NONE',  ( -1.642561882922479732, 10.37072757624895303, 12.29999999999997762 ) ) ;
#4186 = EDGE_CURVE ( 'NONE', #6635, #1178, #7720, .T. ) ;
#4187 = CARTESIAN_POINT ( 'NONE',  ( -13.21436662431716869, 4.623906867372262752, 11.57142857142857295 ) ) ;
#4188 = CARTESIAN_POINT ( 'NONE',  ( -13.51115193377584589, -4.865839792409295761, 24.92453085894499765 ) ) ;
#4189 = ORIENTED_EDGE ( 'NONE', *, *, #2922, .F. ) ;
#4190 = CARTESIAN_POINT ( 'NONE',  ( -10.37072757624895836, 1.642561882922380034, 14.69999999999999041 ) ) ;
#4191 = CARTESIAN_POINT ( 'NONE',  ( -15.89939535829186923, -1.791431617653016062, 17.14285714285713880 ) ) ;
#4192 = DIRECTION ( 'NONE',  ( 1.000000000000000000, -4.575525868300071581E-16, -0.000000000000000000 ) ) ;
#4193 = CARTESIAN_POINT ( 'NONE',  ( -11.78653521626494793, -7.556039541191465148, 42.71024514465928235 ) ) ;
#4194 = CARTESIAN_POINT ( 'NONE',  ( 9.814260835641038128, -5.056896391392198709, 18.35113791807858519 ) ) ;
#4195 = CARTESIAN_POINT ( 'NONE',  ( -1.595456901104623348, 10.37818827243067155, 5.301137918078554279 ) ) ;
#4196 = CARTESIAN_POINT ( 'NONE',  ( 4.200000000000009059, 0.000000000000000000, 0.000000000000000000 ) ) ;
#4197 = CARTESIAN_POINT ( 'NONE',  ( 14.25515036105622535, -1.737328882695210241, 18.36118342676929771 ) ) ;
#4198 = CARTESIAN_POINT ( 'NONE',  ( 7.556039541191335474, 11.78653521626503320, 23.28975485534072121 ) ) ;
#4199 = DIRECTION ( 'NONE',  ( 0.000000000000000000, -6.338944243255235518E-49, 1.000000000000000000 ) ) ;
#4200 = CARTESIAN_POINT ( 'NONE',  ( 5.297344310588354865, 15.53355953199867301, 9.067388001802141773 ) ) ;
#4201 = LINE ( 'NONE', #4104, #2527 ) ;
#4202 = CARTESIAN_POINT ( 'NONE',  ( -1.925929944387235853E-31, -1.018491042385001544, -1.270000000000007123 ) ) ;
#4203 = CARTESIAN_POINT ( 'NONE',  ( 1.612135949262739398, 9.858066664633913234, 8.451137918078549305 ) ) ;
#4204 = CARTESIAN_POINT ( 'NONE',  ( -4.534861676072319270, 8.900167166472121139, 15.14999999999998259 ) ) ;
#4205 = CARTESIAN_POINT ( 'NONE',  ( -162.9192246874586374, 0.5591847127235903825, 12.98870223168555604 ) ) ;
#4206 = CARTESIAN_POINT ( 'NONE',  ( -13.91197093850538380, -1.567502665446387278, 35.14285714285713880 ) ) ;
#4207 = ADVANCED_FACE ( 'NONE', ( #4754 ), #9623, .F. ) ;
#4208 = CARTESIAN_POINT ( 'NONE',  ( -9.899494936611716867, 9.899494936611610285, 36.00000000000000711 ) ) ;
#4209 = VERTEX_POINT ( 'NONE', #2424 ) ;
#4210 = CARTESIAN_POINT ( 'NONE',  ( 13.54758718765249803, 8.512513224245457977, 25.71428571428571885 ) ) ;
#4211 = DIRECTION ( 'NONE',  ( 0.7063021515967569108, 0.7063021515967621289, -0.04769215134145721874 ) ) ;
#4212 = CARTESIAN_POINT ( 'NONE',  ( -15.10213328493390961, 5.284464991282586510, 11.57142857142857295 ) ) ;
#4213 = DIRECTION ( 'NONE',  ( 1.000000000000000000, 4.755747939841215952E-17, -0.000000000000000000 ) ) ;
#4214 = CARTESIAN_POINT ( 'NONE',  ( 4.579542530753127672, -8.877401133907071085, 14.64886208192141659 ) ) ;
#4215 = CARTESIAN_POINT ( 'NONE',  ( 1.677562661911645714, 10.91227292449347175, 16.44886208192140131 ) ) ;
#4216 = UNCERTAINTY_MEASURE_WITH_UNIT (LENGTH_MEASURE( 1.000000000000000082E-05 ), #3524, 'distance_accuracy_value', 'NONE');
#4217 = CARTESIAN_POINT ( 'NONE',  ( -13.82664651025767100, 8.841785722321537477, 15.78975485534072121 ) ) ;
#4218 = CARTESIAN_POINT ( 'NONE',  ( 16.30827793483735633, -1.837501619626142890, 26.35714285714285765 ) ) ;
#4219 = EDGE_CURVE ( 'NONE', #5716, #5081, #2470, .T. ) ;
#4220 = SURFACE_STYLE_USAGE ( .BOTH. , #2569 ) ;
#4221 = CARTESIAN_POINT ( 'NONE',  ( -5.164528828830334817, 15.14410076328347543, 4.432611998197859116 ) ) ;
#4222 = PRODUCT_RELATED_PRODUCT_CATEGORY ( 'part', '', ( #9883 ) ) ;
#4223 = CARTESIAN_POINT ( 'NONE',  ( 14.26974319298268767, -1.607813917172876916, 8.357142857142855874 ) ) ;
#4224 = DIRECTION ( 'NONE',  ( 1.000000000000000000, 0.000000000000000000, 0.000000000000000000 ) ) ;
#4225 = CARTESIAN_POINT ( 'NONE',  ( 4.724406229267374968, 9.377220287599055126, 4.598862081921435419 ) ) ;
#4226 = ORIENTED_EDGE ( 'NONE', *, *, #8698, .F. ) ;
#4227 = CARTESIAN_POINT ( 'NONE',  ( 13.91197093850538380, 1.567502665446386390, 14.14285714285714413 ) ) ;
#4228 = CARTESIAN_POINT ( 'NONE',  ( 13.54758718765249803, 8.512513224245457977, 31.71428571428571530 ) ) ;
#4229 = CARTESIAN_POINT ( 'NONE',  ( 8.404922754268618235, 13.61519076058357491, 33.28167371608784464 ) ) ;
#4230 = CARTESIAN_POINT ( 'NONE',  ( -10.90442828429183919, -1.727091770866655329, 5.549999999999999822 ) ) ;
#4231 = CARTESIAN_POINT ( 'NONE',  ( 13.21436662431716869, -4.623906867372263640, 14.57142857142856940 ) ) ;
#4232 = CARTESIAN_POINT ( 'NONE',  ( -11.78653521626494793, -7.556039541191465148, 24.71024514465928235 ) ) ;
#4233 = FILL_AREA_STYLE ('',( #8159 ) ) ;
#4234 = B_SPLINE_CURVE_WITH_KNOTS ( 'NONE', 3,
 ( #4938, #4262, #1016, #6372, #2607, #7312, #8037, #2560, #288, #185, #236, #9550, #2509, #5751, #4991, #6520, #1069, #1739, #5803, #8980, #5658, #6424, #2457, #5603, #9699, #1694, #8768, #4835, #4064, #8919, #7211, #9605, #8826, #4889, #964, #9849, #6618, #6050, #4362, #9180, #4465, #8389, #2707, #9074, #3633, #2907, #8339, #3582, #1257, #338, #4522, #9225, #7621, #7515, #4416, #1312, #2141, #542 ),
 .UNSPECIFIED., .F., .F.,
 ( 4, 2, 2, 2, 2, 2, 2, 2, 2, 2, 2, 2, 2, 2, 2, 2, 2, 2, 2, 2, 2, 2, 2, 2, 2, 2, 2, 2, 4 ),
 ( 0.000000000000000000, 0.002013233252797604154, 0.004026466505595208308, 0.006039699758392812895, 0.008052933011190416615, 0.01207939951678562579, 0.01308601614318442678, 0.01409263276958323124, 0.01459594108278263087, 0.01484759523938233156, 0.01497342231768217929, 0.01503633585683210490, 0.01509924939598203050, 0.01516216293513195611, 0.01522507647428187998, 0.01535090355258173465, 0.01560255770918144401, 0.01610586602238086099, 0.01711248264877969841, 0.01811909927517853583, 0.02013233252797621067, 0.02113894915437504810, 0.02214556578077388899, 0.02415879903357156383, 0.02516541565997040125, 0.02617203228636923867, 0.02818526553916691699, 0.03019849879196460224, 0.03221173204476228402 ),
 .UNSPECIFIED. ) ;
#4235 = DIRECTION ( 'NONE',  ( 1.000000000000000000, -4.575525868300071581E-16, -0.000000000000000000 ) ) ;
#4236 = EDGE_CURVE ( 'NONE', #6181, #6566, #7850, .T. ) ;
#4237 = CARTESIAN_POINT ( 'NONE',  ( -1.737328882695368115, 14.25515036105620581, 32.63881657323070584 ) ) ;
#4238 = CARTESIAN_POINT ( 'NONE',  ( 4.766900247265192903, 9.355568503977902850, 0.5999999999999894307 ) ) ;
#4239 = CARTESIAN_POINT ( 'NONE',  ( -10.36326688006724162, 1.689666864740235308, 7.701137918078540423 ) ) ;
#4240 = AXIS2_PLACEMENT_3D ( 'NONE', #7680, #3116, #9438 ) ;
#4241 = EDGE_CURVE ( 'NONE', #6181, #6566, #9457, .T. ) ;
#4242 = DIRECTION ( 'NONE',  ( 0.000000000000000000, 1.224646799147353207E-16, 1.000000000000000000 ) ) ;
#4243 = CARTESIAN_POINT ( 'NONE',  ( -7.529642458189277576, 12.22833218042435455, 22.21832628391215181 ) ) ;
#4244 = CARTESIAN_POINT ( 'NONE',  ( -12.08964793087886314, 7.750357176954159932, 27.78975485534072121 ) ) ;
#4245 = CARTESIAN_POINT ( 'NONE',  ( -10.90442828429183919, -1.727091770866654663, 11.54999999999998295 ) ) ;
#4246 = CARTESIAN_POINT ( 'NONE',  ( 8.841785722321695573, -13.82664651025757152, 35.21024514465927524 ) ) ;
#4247 = ORIENTED_EDGE ( 'NONE', *, *, #7128, .F. ) ;
#4248 = CARTESIAN_POINT ( 'NONE',  ( -11.67616201620524130, 10.40597831933767736, 48.73000000000001108 ) ) ;
#4249 = CARTESIAN_POINT ( 'NONE',  ( 15.49051278174638036, 5.420364854932175014, 19.92857142857143771 ) ) ;
#4250 = CARTESIAN_POINT ( 'NONE',  ( -15.14410076328353227, 5.164528828830164287, 13.56738800180213822 ) ) ;
#4251 = CARTESIAN_POINT ( 'NONE',  ( -166.6500000000000057, -0.2154325771598549211, 13.00000000000000533 ) ) ;
#4252 = CYLINDRICAL_SURFACE ( 'NONE', #2153, 0.9906000000000003691 ) ;
#4253 = STYLED_ITEM ( 'NONE', ( #7960 ), #939 ) ;
#4254 = CARTESIAN_POINT ( 'NONE',  ( -8.877401133907129704, 4.579542530753042406, 4.851137918078532785 ) ) ;
#4255 = CARTESIAN_POINT ( 'NONE',  ( -8.900167166472156666, 4.534861676072231340, 14.84999999999999787 ) ) ;
#4256 = CARTESIAN_POINT ( 'NONE',  ( -166.7097254823910077, 1.311132300232774162, 14.94304721624505028 ) ) ;
#4257 = CARTESIAN_POINT ( 'NONE',  ( 1.567502665446232957, 13.91197093850540156, 36.85714285714286120 ) ) ;
#4258 = CARTESIAN_POINT ( 'NONE',  ( -1.567502665446231180, -13.91197093850540334, 33.85714285714285410 ) ) ;
#4259 = ORIENTED_EDGE ( 'NONE', *, *, #290, .T. ) ;
#4260 = ADVANCED_BREP_SHAPE_REPRESENTATION ( '', ( #3605, #3995 ), #8889 ) ;
#4261 = CARTESIAN_POINT ( 'NONE',  ( -5.404401153735176599, 15.06016580658422477, 2.424530858944988321 ) ) ;
#4262 = CARTESIAN_POINT ( 'NONE',  ( -9.423904007443638875, 10.37508586577969183, -0.000000000000000000 ) ) ;
#4263 = CARTESIAN_POINT ( 'NONE',  ( -13.54758718765249625, -8.512513224245459753, 22.71428571428571530 ) ) ;
#4264 = ADVANCED_FACE ( 'NONE', ( #2577 ), #7069, .T. ) ;
#4265 = PRODUCT_DEFINITION_SHAPE ( 'NONE', 'NONE',  #10230 ) ;
#4266 = CARTESIAN_POINT ( 'NONE',  ( 8.442910196168311288, 4.355403765523574222, 19.89886208192141481 ) ) ;
#4267 = CARTESIAN_POINT ( 'NONE',  ( -6.751237864895158758, 6.683790977649260334, 9.998862081921425116 ) ) ;
#4268 = CARTESIAN_POINT ( 'NONE',  ( -11.22385875690717327, 11.40355824106234550, 4.004040569626432067 ) ) ;
#4269 = CARTESIAN_POINT ( 'NONE',  ( -1.837501619626328297, 16.30827793483733856, 30.64285714285715301 ) ) ;
#4270 = EDGE_CURVE ( 'NONE', #1499, #3063, #4003, .T. ) ;
#4271 = CARTESIAN_POINT ( 'NONE',  ( -5.164528828830334817, 15.14410076328347543, 10.43261199819786356 ) ) ;
#4272 = CARTESIAN_POINT ( 'NONE',  ( -12.15899005565164792, 7.639999817571651697, 29.78571428571428825 ) ) ;
#4273 = CARTESIAN_POINT ( 'NONE',  ( -5.420364854931999155, -15.49051278174644253, 4.071428571428569398 ) ) ;
#4274 = CARTESIAN_POINT ( 'NONE',  ( 10.37818827243067510, -1.595456901104500780, 5.198862081921453715 ) ) ;
#4275 = EDGE_LOOP ( 'NONE', ( #5969, #1863, #9950 ) ) ;
#4276 = CARTESIAN_POINT ( 'NONE',  ( -13.21436662431716869, 4.623906867372262752, 23.57142857142857650 ) ) ;
#4277 = ORIENTED_EDGE ( 'NONE', *, *, #4838, .F. ) ;
#4278 = CARTESIAN_POINT ( 'NONE',  ( 16.30827793483735633, -1.837501619626142890, 32.35714285714286120 ) ) ;
#4279 = CARTESIAN_POINT ( 'NONE',  ( -1.737328882695368115, 14.25515036105620581, 2.638816573230710727 ) ) ;
#4280 = CARTESIAN_POINT ( 'NONE',  ( 5.012215536711511987, -9.837026868205999364, 10.65000000000000924 ) ) ;
#4281 = CARTESIAN_POINT ( 'NONE',  ( 14.26974319298268767, -1.607813917172876472, 8.357142857142855874 ) ) ;
#4282 = ORIENTED_EDGE ( 'NONE', *, *, #429, .F. ) ;
#4283 = CARTESIAN_POINT ( 'NONE',  ( -13.51115193377584589, -4.865839792409295761, 30.92453085894499765 ) ) ;
#4284 =( GEOMETRIC_REPRESENTATION_CONTEXT ( 3 ) GLOBAL_UNCERTAINTY_ASSIGNED_CONTEXT ( ( #5854 ) ) GLOBAL_UNIT_ASSIGNED_CONTEXT ( ( #5086, #187, #238 ) ) REPRESENTATION_CONTEXT ( 'NONE', 'WORKASPACE' ) );
#4285 = SURFACE_STYLE_USAGE ( .BOTH. , #1913 ) ;
#4286 = CARTESIAN_POINT ( 'NONE',  ( 4.398722002148208077, 13.35545020628939739, 48.73000000000001819 ) ) ;
#4287 = CARTESIAN_POINT ( 'NONE',  ( 1.677562661911645714, 10.91227292449347175, 16.44886208192140131 ) ) ;
#4288 = CARTESIAN_POINT ( 'NONE',  ( -7.842167650704559456, -7.771249796623176387, 10.25113791807858021 ) ) ;
#4289 = CARTESIAN_POINT ( 'NONE',  ( 10.36326688006723984, -1.689666864740212215, 0.2011379180785754783 ) ) ;
#4290 = PLANE ( 'NONE',  #4803 ) ;
#4291 = CARTESIAN_POINT ( 'NONE',  ( -10.24623928997352351, -10.06191849875416899, 20.50404056962644006 ) ) ;
#4292 = AXIS2_PLACEMENT_3D ( 'NONE', #1734, #8866, #1779 ) ;
#4293 =( NAMED_UNIT ( * ) SI_UNIT ( $, .STERADIAN. ) SOLID_ANGLE_UNIT ( ) );
#4294 = CARTESIAN_POINT ( 'NONE',  ( 1.693770420379222319, 13.89774397934251837, 22.86118342676929061 ) ) ;
#4295 = CARTESIAN_POINT ( 'NONE',  ( -9.355568503977838901, -4.766900247265279944, 5.400000000000016342 ) ) ;
#4296 = CARTESIAN_POINT ( 'NONE',  ( -15.88516839912898071, -1.917699372586004980, 43.13881657323070584 ) ) ;
#4297 = CARTESIAN_POINT ( 'NONE',  ( -12.16676467619702606, 8.075659364407771434, 48.73000000000002530 ) ) ;
#4298 = CARTESIAN_POINT ( 'NONE',  ( -5.420364854931999155, -15.49051278174644253, 22.07142857142858006 ) ) ;
#4299 = CARTESIAN_POINT ( 'NONE',  ( 1.665163862719847732, 15.91362231745477374, 2.853102287516426916 ) ) ;
#4300 = CARTESIAN_POINT ( 'NONE',  ( -163.3500000000000512, -1.154202410357457390E-14, 13.00000000000000355 ) ) ;
#4301 = VECTOR ( 'NONE', #6221, 1000.000000000000000 ) ;
#4302 = CIRCLE ( 'NONE', #6441, 0.4999999999999994449 ) ;
#4303 = CONICAL_SURFACE ( 'NONE', #6934, 1.610000000000000098, 0.7853981633974658205 ) ;
#4304 = CARTESIAN_POINT ( 'NONE',  ( 4.355403765523470305, 8.442910196168369907, 5.601137918078562983 ) ) ;
#4305 = CARTESIAN_POINT ( 'NONE',  ( 9.865911304835474738, 1.562606840307950051, 16.04999999999995808 ) ) ;
#4306 = DIRECTION ( 'NONE',  ( 1.000000000000000000, 0.000000000000000000, 0.000000000000000000 ) ) ;
#4307 = CARTESIAN_POINT ( 'NONE',  ( 13.91197093850538380, 1.567502665446386390, 26.14285714285714590 ) ) ;
#4308 = CIRCLE ( 'NONE', #7941, 16.00000000000000000 ) ;
#4309 = AXIS2_PLACEMENT_3D ( 'NONE', #6311, #10154, #3949 ) ;
#4310 = CIRCLE ( 'NONE', #2496, 16.00000000000000000 ) ;
#4311 = CARTESIAN_POINT ( 'NONE',  ( 7.448449071214646722, 11.85413878919601594, 43.28571428571429180 ) ) ;
#4312 = ORIENTED_EDGE ( 'NONE', *, *, #74, .F. ) ;
#4313 = CARTESIAN_POINT ( 'NONE',  ( 1.791431617652837316, 15.89939535829188877, 42.85714285714285410 ) ) ;
#4314 = DIRECTION ( 'NONE',  ( 0.000000000000000000, -6.338944243255235518E-49, 1.000000000000000000 ) ) ;
#4315 = CARTESIAN_POINT ( 'NONE',  ( -8.731428362939189114, 13.89598863503036341, 12.21428571428571885 ) ) ;
#4316 = ADVANCED_FACE ( 'NONE', ( #4802 ), #8796, .F. ) ;
#4317 = CARTESIAN_POINT ( 'NONE',  ( -162.8500000000000512, -5.808233151972152598E-15, 15.00000000000000000 ) ) ;
#4318 = CARTESIAN_POINT ( 'NONE',  ( -1.486127417882243895, 9.383039235653816590, 0.2999999999999669598 ) ) ;
#4319 = CARTESIAN_POINT ( 'NONE',  ( -4.270415729527831772, -8.486213763410670907, 6.098862081921437195 ) ) ;
#4320 = UNCERTAINTY_MEASURE_WITH_UNIT (LENGTH_MEASURE( 1.000000000000000082E-05 ), #2333, 'distance_accuracy_value', 'NONE');
#4321 = CARTESIAN_POINT ( 'NONE',  ( -5.543385399275643444, -15.44746603149420494, 14.07546914105500768 ) ) ;
#4322 = CARTESIAN_POINT ( 'NONE',  ( -13.54758718765249625, -8.512513224245459753, 22.71428571428571530 ) ) ;
#4323 = CARTESIAN_POINT ( 'NONE',  ( -11.22385875690717327, 11.40355824106234550, 10.00404056962643651 ) ) ;
#4324 = CARTESIAN_POINT ( 'NONE',  ( -9.899494936611716867, 9.899494936611610285, 30.00000000000000355 ) ) ;
#4325 = CARTESIAN_POINT ( 'NONE',  ( -13.89598863503046111, 8.731428362939027465, 11.78571428571428115 ) ) ;
#4326 = CARTESIAN_POINT ( 'NONE',  ( -68.00000000000002842, 0.000000000000000000, 0.000000000000000000 ) ) ;
#4327 = EDGE_LOOP ( 'NONE', ( #9574, #5316 ) ) ;
#4328 = CARTESIAN_POINT ( 'NONE',  ( 1.567502665446232957, 13.91197093850540156, 18.85714285714285765 ) ) ;
#4329 = ORIENTED_EDGE ( 'NONE', *, *, #8243, .F. ) ;
#4330 = CARTESIAN_POINT ( 'NONE',  ( -1.837501619626327853, 16.30827793483733856, 36.64285714285714590 ) ) ;
#4331 = CARTESIAN_POINT ( 'NONE',  ( 13.51115193377584589, 4.865839792409294873, 3.924530858944990541 ) ) ;
#4332 = CARTESIAN_POINT ( 'NONE',  ( 10.37072757624895836, -1.642561882922355831, 19.19999999999999574 ) ) ;
#4333 = CARTESIAN_POINT ( 'NONE',  ( -165.0000000000000284, -6.071532165918824830E-15, 18.99999999999997868 ) ) ;
#4334 = CARTESIAN_POINT ( 'NONE',  ( 1.567502665446232957, 13.91197093850540156, 6.857142857142860315 ) ) ;
#4335 = CARTESIAN_POINT ( 'NONE',  ( 14.28433602490915000, -1.478298951650544479, 28.35310228751642825 ) ) ;
#4336 =( NAMED_UNIT ( * ) PLANE_ANGLE_UNIT ( ) SI_UNIT ( $, .RADIAN. ) );
#4337 = CARTESIAN_POINT ( 'NONE',  ( -166.4312272284851986, 0.8280293812990602298, 12.97391163473193387 ) ) ;
#4338 = APPLICATION_CONTEXT ( 'automotive_design' ) ;
#4339 = CARTESIAN_POINT ( 'NONE',  ( 9.390499931835536884, -1.439022436064273158, 5.198862081921453715 ) ) ;
#4340 = CARTESIAN_POINT ( 'NONE',  ( 12.15899005565164792, -7.639999817571655250, 2.785714285714284255 ) ) ;
#4341 = CARTESIAN_POINT ( 'NONE',  ( 10.37072757624895836, -1.642561882922355609, 7.199999999999984190 ) ) ;
#4342 = CARTESIAN_POINT ( 'NONE',  ( -9.377220287598998283, -4.724406229267462898, 1.401137918078568134 ) ) ;
#4343 = CARTESIAN_POINT ( 'NONE',  ( -2.000000000000001776, -9.511495879682425741E-17, 0.000000000000000000 ) ) ;
#4344 = CARTESIAN_POINT ( 'NONE',  ( 13.17239914596754424, -4.743843029824685864, 30.57546914105500946 ) ) ;
#4345 = CARTESIAN_POINT ( 'NONE',  ( -11.92174236212692051, -7.340858601238089420, 20.71832628391214826 ) ) ;
#4346 = PRODUCT_DEFINITION ( 'UNKNOWN', '', #9394, #494 ) ;
#4347 = CARTESIAN_POINT ( 'NONE',  ( -7.806708723663830618, -7.806708723663906113, 8.250000000000028422 ) ) ;
#4348 = CARTESIAN_POINT ( 'NONE',  ( -8.841785722321695573, 13.82664651025757152, 38.21024514465928235 ) ) ;
#4349 = CARTESIAN_POINT ( 'NONE',  ( -10.03741027250566020, 10.21278494640099588, 48.73000000000001819 ) ) ;
#4350 = CARTESIAN_POINT ( 'NONE',  ( -1.837501619626328297, 16.30827793483733856, 24.64285714285714235 ) ) ;
#4351 = CARTESIAN_POINT ( 'NONE',  ( -58.00000000000001421, 0.000000000000000000, 0.000000000000000000 ) ) ;
#4352 = AXIS2_PLACEMENT_3D ( 'NONE', #6148, #7768, #7815 ) ;
#4353 = CARTESIAN_POINT ( 'NONE',  ( -13.51115193377584589, -4.865839792409295761, 12.92453085894499587 ) ) ;
#4354 = CARTESIAN_POINT ( 'NONE',  ( -6.683790977649319842, 6.751237864895101026, 8.001137918078546463 ) ) ;
#4355 = CARTESIAN_POINT ( 'NONE',  ( 8.486213763410640709, 4.270415729527937465, -0.09886208192143307316 ) ) ;
#4356 = CARTESIAN_POINT ( 'NONE',  ( -2.000000000000001776, -9.511495879682425741E-17, 0.000000000000000000 ) ) ;
#4357 = CARTESIAN_POINT ( 'NONE',  ( 8.620103694221997515, 13.47998361472160767, 35.28975485534072476 ) ) ;
#4358 = CARTESIAN_POINT ( 'NONE',  ( 1.567502665446232957, 13.91197093850540156, 30.85714285714286120 ) ) ;
#4359 = CARTESIAN_POINT ( 'NONE',  ( -1.567502665446231180, -13.91197093850540334, 39.85714285714286120 ) ) ;
#4360 = EDGE_LOOP ( 'NONE', ( #3231, #5060, #5358, #3708 ) ) ;
#4361 = CARTESIAN_POINT ( 'NONE',  ( -13.54758718765249625, -8.512513224245459753, 46.71428571428571530 ) ) ;
#4362 = CARTESIAN_POINT ( 'NONE',  ( 1.550455870813287396, 15.46333760686143144, 9.306676823330681010E-17 ) ) ;
#4363 = CARTESIAN_POINT ( 'NONE',  ( -16.30827793483735988, 1.837501619626141780, 35.35714285714285410 ) ) ;
#4364 = CARTESIAN_POINT ( 'NONE',  ( -158.0000000000000284, -7.514081744949122117E-15, 0.000000000000000000 ) ) ;
#4365 = CARTESIAN_POINT ( 'NONE',  ( -108.0000000000000284, 0.000000000000000000, 0.000000000000000000 ) ) ;
#4366 = EDGE_CURVE ( 'NONE', #2935, #5915, #1604, .T. ) ;
#4367 = CARTESIAN_POINT ( 'NONE',  ( 6.919986107680329290, -12.02850919814119379, -1.270000000000007123 ) ) ;
#4368 = CARTESIAN_POINT ( 'NONE',  ( 8.922933199037192509, -4.490180821391404287, 20.34886208192140700 ) ) ;
#4369 = CARTESIAN_POINT ( 'NONE',  ( -4.579542530753125895, 8.877401133907090625, 10.14886208192142725 ) ) ;
#4370 = CARTESIAN_POINT ( 'NONE',  ( -9.355568503977838901, -4.766900247265280832, 14.39999999999996838 ) ) ;
#4371 = EDGE_CURVE ( 'NONE', #9073, #8249, #6614, .T. ) ;
#4372 = CARTESIAN_POINT ( 'NONE',  ( 15.06016580658428694, -5.404401153735007846, 6.575469141055007682 ) ) ;
#4373 = CARTESIAN_POINT ( 'NONE',  ( 15.89939535829187278, 1.791431617653015174, 26.14285714285714590 ) ) ;
#4374 = ADVANCED_FACE ( 'NONE', ( #3249 ), #931, .T. ) ;
#4375 = CARTESIAN_POINT ( 'NONE',  ( 13.82664651025767100, -8.841785722321541030, 12.78975485534072121 ) ) ;
#4376 = CARTESIAN_POINT ( 'NONE',  ( -4.623906867372410190, 13.21436662431711895, 18.42857142857143415 ) ) ;
#4377 = CARTESIAN_POINT ( 'NONE',  ( -8.731428362939189114, 13.89598863503036341, 6.214285714285717965 ) ) ;
#4378 = CARTESIAN_POINT ( 'NONE',  ( -16.30827793483735988, 1.837501619626141780, 41.35714285714286120 ) ) ;
#4379 = ORIENTED_EDGE ( 'NONE', *, *, #1870, .T. ) ;
#4380 = CARTESIAN_POINT ( 'NONE',  ( -4.623906867372410190, 13.21436662431711895, 12.42857142857142705 ) ) ;
#4381 = DIRECTION ( 'NONE',  ( -1.000000000000000000, 0.000000000000000000, 0.000000000000000000 ) ) ;
#4382 = CARTESIAN_POINT ( 'NONE',  ( -16.30827793483735988, 1.837501619626141558, 35.35714285714286120 ) ) ;
#4383 = CARTESIAN_POINT ( 'NONE',  ( 4.743843029824831525, -13.17239914596749095, 5.424530858944991429 ) ) ;
#4384 = CARTESIAN_POINT ( 'NONE',  ( 1.642561882922480621, -10.37072757624892638, 13.80000000000003446 ) ) ;
#4385 = PRODUCT_CONTEXT ( 'NONE', #4338, 'mechanical' ) ;
#4386 = CARTESIAN_POINT ( 'NONE',  ( -14.26974319298268767, 1.607813917172874696, 5.357142857142856762 ) ) ;
#4387 = EDGE_LOOP ( 'NONE', ( #3755, #930 ) ) ;
#4388 = CARTESIAN_POINT ( 'NONE',  ( -13.25633410266679313, 4.503970704919840529, 25.56738800180213644 ) ) ;
#4389 = ORIENTED_EDGE ( 'NONE', *, *, #7622, .T. ) ;
#4390 = SURFACE_STYLE_USAGE ( .BOTH. , #3514 ) ;
#4391 = DIRECTION ( 'NONE',  ( 0.000000000000000000, 0.000000000000000000, 1.000000000000000000 ) ) ;
#4392 = ADVANCED_FACE ( 'NONE', ( #9287, #2858 ), #1259, .T. ) ;
#4393 = CARTESIAN_POINT ( 'NONE',  ( 1.513077731352925115, 9.873755945037103743, 1.448862081921441947 ) ) ;
#4394 = CARTESIAN_POINT ( 'NONE',  ( 1.737328882695370558, -14.25515036105620581, 47.63881657323071295 ) ) ;
#4395 = CARTESIAN_POINT ( 'NONE',  ( 1.642561882922480621, -10.37072757624892638, 4.800000000000026468 ) ) ;
#4396 = CARTESIAN_POINT ( 'NONE',  ( -1.595456901104623348, 10.37818827243066622, 2.301137918078551614 ) ) ;
#4397 = DIRECTION ( 'NONE',  ( 0.000000000000000000, 1.000000000000000000, -1.224646799147353207E-16 ) ) ;
#4398 = CARTESIAN_POINT ( 'NONE',  ( 13.92619789766827587, 1.441234910513398582, 30.14689771248358241 ) ) ;
#4399 = FILL_AREA_STYLE_COLOUR ( '', #6125 ) ;
#4400 = CARTESIAN_POINT ( 'NONE',  ( -4.766900247265192014, -9.355568503977867323, 8.099999999999996092 ) ) ;
#4401 = CARTESIAN_POINT ( 'NONE',  ( -5.404401153735176599, 15.06016580658422477, 38.42453085894499054 ) ) ;
#4402 = CARTESIAN_POINT ( 'NONE',  ( -8.450287677708004708, 11.41786575994333042, 48.73000000000001819 ) ) ;
#4403 = CARTESIAN_POINT ( 'NONE',  ( 11.60466159355862104, 11.60466159355875071, 19.50000000000000355 ) ) ;
#4404 = LINE ( 'NONE', #6040, #5659 ) ;
#4405 = CIRCLE ( 'NONE', #2742, 18.00000000000001776 ) ;
#4406 = CARTESIAN_POINT ( 'NONE',  ( -10.06191849875405531, -10.24623928997363542, 18.49595943037356705 ) ) ;
#4407 = CARTESIAN_POINT ( 'NONE',  ( -9.375578539472099848, 1.533232399700010351, 16.70113791807854398 ) ) ;
#4408 = CARTESIAN_POINT ( 'NONE',  ( -1.486127417882243895, 9.383039235653816590, 18.29999999999998295 ) ) ;
#4409 = EDGE_CURVE ( 'NONE', #1541, #8205, #2909, .T. ) ;
#4410 = DIRECTION ( 'NONE',  ( 0.000000000000000000, -6.338944243255235518E-49, 1.000000000000000000 ) ) ;
#4411 = CARTESIAN_POINT ( 'NONE',  ( -7.529642458189277576, 12.22833218042435455, -1.781673716087850634 ) ) ;
#4412 = CIRCLE ( 'NONE', #7052, 2.000000000000000888 ) ;
#4413 = CARTESIAN_POINT ( 'NONE',  ( -13.91197093850538380, -1.567502665446387278, 35.14285714285713880 ) ) ;
#4414 = ORIENTED_EDGE ( 'NONE', *, *, #3789, .F. ) ;
#4415 = CARTESIAN_POINT ( 'NONE',  ( -11.40355824106246807, 11.22385875690704715, 1.995959430373561272 ) ) ;
#4416 = CARTESIAN_POINT ( 'NONE',  ( -9.315939868251517098, 13.01050362062812660, 4.615094676506724096E-15 ) ) ;
#4417 = CARTESIAN_POINT ( 'NONE',  ( 5.420364854932001819, 15.49051278174644430, 31.07142857142857295 ) ) ;
#4418 = LINE ( 'NONE', #5193, #2345 ) ;
#4419 = DIRECTION ( 'NONE',  ( 0.000000000000000000, 6.938893903907221444E-18, 1.000000000000000000 ) ) ;
#4420 = DIRECTION ( 'NONE',  ( 0.000000000000000000, 0.4999999999999991673, -0.8660254037844390407 ) ) ;
#4421 = CARTESIAN_POINT ( 'NONE',  ( -8.900167166472156666, 4.534861676072231340, 2.849999999999968114 ) ) ;
#4422 = CARTESIAN_POINT ( 'NONE',  ( -1.513077731352923339, -9.873755945037078874, 11.94886208192145993 ) ) ;
#4423 = PRODUCT_DEFINITION_CONTEXT ( 'detailed design', #6570, 'design' ) ;
#4424 = CARTESIAN_POINT ( 'NONE',  ( 9.837026868206066865, -5.012215536711395636, 16.35000000000000497 ) ) ;
#4425 = CARTESIAN_POINT ( 'NONE',  ( 1.707986654103998303, -16.32287076676380266, 13.64689771248357708 ) ) ;
#4426 = CARTESIAN_POINT ( 'NONE',  ( -8.512513224245306986, -13.54758718765259218, 40.28571428571428470 ) ) ;
#4427 = MECHANICAL_DESIGN_GEOMETRIC_PRESENTATION_REPRESENTATION (  '', ( #4095 ), #3103 ) ;
#4428 = CARTESIAN_POINT ( 'NONE',  ( 1.707986654103998303, -16.32287076676380266, 1.646897712483578857 ) ) ;
#4429 = CARTESIAN_POINT ( 'NONE',  ( -10.15407889436378852, -10.15407889436390576, 28.50000000000001066 ) ) ;
#4430 = CARTESIAN_POINT ( 'NONE',  ( -5.284464991282755264, 15.10213328493384743, 6.428571428571429713 ) ) ;
#4431 = CARTESIAN_POINT ( 'NONE',  ( 11.31370849898469899, 11.31370849898481978, 49.50000000000000711 ) ) ;
#4432 = ORIENTED_EDGE ( 'NONE', *, *, #7927, .F. ) ;
#4433 = CARTESIAN_POINT ( 'NONE',  ( 7.424621202458790314, -7.424621202458697944, 10.50000000000000888 ) ) ;
#4434 = EDGE_CURVE ( 'NONE', #3839, #1952, #6052, .T. ) ;
#4435 = EDGE_LOOP ( 'NONE', ( #515, #465 ) ) ;
#4436 = PRODUCT_DEFINITION_FORMATION_WITH_SPECIFIED_SOURCE ( 'ANY', '', #9805, .NOT_KNOWN. ) ;
#4437 = CARTESIAN_POINT ( 'NONE',  ( -11.31370849898482156, 11.31370849898469544, 30.00000000000000355 ) ) ;
#4438 = CARTESIAN_POINT ( 'NONE',  ( -7.340858601237953529, -11.92174236212700222, 6.281673716087846415 ) ) ;
#4439 = CARTESIAN_POINT ( 'NONE',  ( -10.90442828429183919, -1.727091770866654663, 17.55000000000002913 ) ) ;
#4440 = SHAPE_DEFINITION_REPRESENTATION ( #5823, #3478 ) ;
#4441 = CARTESIAN_POINT ( 'NONE',  ( 14.26974319298268767, -1.607813917172876472, 20.35714285714285765 ) ) ;
#4442 = CARTESIAN_POINT ( 'NONE',  ( -1.441234910513241818, -13.92619789766829008, 35.85310228751641404 ) ) ;
#4443 = ORIENTED_EDGE ( 'NONE', *, *, #2412, .F. ) ;
#4444 = DIRECTION ( 'NONE',  ( -1.000000000000000000, -0.000000000000000000, -0.000000000000000000 ) ) ;
#4445 = CARTESIAN_POINT ( 'NONE',  ( -1.533232399700100057, 9.375578539472089190, 4.298862081921427603 ) ) ;
#4446 = CARTESIAN_POINT ( 'NONE',  ( 13.25633410266679313, -4.503970704919842305, 46.56738800180214355 ) ) ;
#4447 = CARTESIAN_POINT ( 'NONE',  ( -9.837026868206066865, 5.012215536711413399, 8.850000000000008527 ) ) ;
#4448 = CARTESIAN_POINT ( 'NONE',  ( 9.814260835641038128, -5.056896391392198709, 9.351137918078563871 ) ) ;
#4449 = CARTESIAN_POINT ( 'NONE',  ( 2.000000000000001776, 1.773042676681366281, 0.000000000000000000 ) ) ;
#4450 = CARTESIAN_POINT ( 'NONE',  ( 12.08964793087886314, -7.750357176954162597, 30.78975485534071765 ) ) ;
#4451 = CARTESIAN_POINT ( 'NONE',  ( -1.727091770866549414, -10.90442828429184630, 13.95000000000002593 ) ) ;
#4452 = CARTESIAN_POINT ( 'NONE',  ( 11.51250119794888249, 11.69682198916847682, 39.49595943037357415 ) ) ;
#4453 = CARTESIAN_POINT ( 'NONE',  ( -12.40202720642545309, 9.316290079762461929, 48.72999999999998266 ) ) ;
#4454 = DIRECTION ( 'NONE',  ( 1.000000000000000000, -4.575525868300071581E-16, -0.000000000000000000 ) ) ;
#4455 = CARTESIAN_POINT ( 'NONE',  ( 12.22833218042443271, -7.529642458189144349, 16.78167371608784819 ) ) ;
#4456 = CARTESIAN_POINT ( 'NONE',  ( -4.490180821391513533, 8.922933199037158758, 11.15113791807855215 ) ) ;
#4457 = CARTESIAN_POINT ( 'NONE',  ( 8.877401133907127928, -4.579542530753020202, 6.351137918078572753 ) ) ;
#4458 = CARTESIAN_POINT ( 'NONE',  ( -166.8657786825345397, 1.077543057910302471, 14.96170541662921316 ) ) ;
#4459 = CARTESIAN_POINT ( 'NONE',  ( 4.623906867372411078, -13.21436662431711717, 45.42857142857143060 ) ) ;
#4460 = CARTESIAN_POINT ( 'NONE',  ( 10.24623928997352884, 10.06191849875416899, 5.504040569626439172 ) ) ;
#4461 = ORIENTED_EDGE ( 'NONE', *, *, #2699, .F. ) ;
#4462 = CIRCLE ( 'NONE', #8425, 1.816100000000000270 ) ;
#4463 = CARTESIAN_POINT ( 'NONE',  ( 15.10213328493390783, -5.284464991282587398, 44.57142857142857650 ) ) ;
#4464 = AXIS2_PLACEMENT_3D ( 'NONE', #4630, #6262, #2252 ) ;
#4465 = CARTESIAN_POINT ( 'NONE',  ( -0.06637551812352288083, 15.68265704790004023, -1.227588689168337064E-16 ) ) ;
#4466 = PRESENTATION_LAYER_ASSIGNMENT (  '', '', ( #1028 ) ) ;
#4467 = VECTOR ( 'NONE', #1673, 1000.000000000000000 ) ;
#4468 = CARTESIAN_POINT ( 'NONE',  ( -15.89939535829186923, -1.791431617653016062, 29.14285714285714235 ) ) ;
#4469 = CARTESIAN_POINT ( 'NONE',  ( 4.246973736992224246, -14.10948682827615919, 0.000000000000000000 ) ) ;
#4470 = FILL_AREA_STYLE ('',( #8293 ) ) ;
#4471 = CARTESIAN_POINT ( 'NONE',  ( -5.012215536711506658, 9.837026868206027785, 0.1499999999999952482 ) ) ;
#4472 = CARTESIAN_POINT ( 'NONE',  ( 1.562606840307832368, 9.865911304835510265, 9.449999999999988631 ) ) ;
#4473 = CARTESIAN_POINT ( 'NONE',  ( 6.751237864895159646, -6.683790977649233689, 8.498862081921462419 ) ) ;
#4474 = CARTESIAN_POINT ( 'NONE',  ( -4.766900247265192014, -9.355568503977876205, 14.10000000000000142 ) ) ;
#4475 = CARTESIAN_POINT ( 'NONE',  ( -13.54758718765249625, -8.512513224245459753, 40.71428571428571530 ) ) ;
#4476 =( GEOMETRIC_REPRESENTATION_CONTEXT ( 3 ) GLOBAL_UNCERTAINTY_ASSIGNED_CONTEXT ( ( #8878 ) ) GLOBAL_UNIT_ASSIGNED_CONTEXT ( ( #8772, #133, #3284 ) ) REPRESENTATION_CONTEXT ( 'NONE', 'WORKASPACE' ) );
#4477 = VECTOR ( 'NONE', #3902, 1000.000000000000000 ) ;
#4478 = CIRCLE ( 'NONE', #3320, 20.00000000000000000 ) ;
#4479 = CARTESIAN_POINT ( 'NONE',  ( -1.917699372585823570, -15.88516839912900558, 25.86118342676929416 ) ) ;
#4480 = CARTESIAN_POINT ( 'NONE',  ( 14.26974319298268767, -1.607813917172876916, 20.35714285714286476 ) ) ;
#4481 = CARTESIAN_POINT ( 'NONE',  ( -13.54758718765249625, -8.512513224245459753, 4.714285714285712636 ) ) ;
#4482 = CARTESIAN_POINT ( 'NONE',  ( 11.31370849898482334, -11.31370849898469366, 45.00000000000000711 ) ) ;
#4483 = EDGE_LOOP ( 'NONE', ( #8536, #1229, #7197, #3978 ) ) ;
#4484 = CARTESIAN_POINT ( 'NONE',  ( 10.90442828429183919, 1.727091770866679532, 19.04999999999997939 ) ) ;
#4485 = ORIENTED_EDGE ( 'NONE', *, *, #3292, .T. ) ;
#4486 = STYLED_ITEM ( 'NONE', ( #5201 ), #8958 ) ;
#4487 = DIRECTION ( 'NONE',  ( 1.000000000000000000, 4.755747939841215952E-17, -0.000000000000000000 ) ) ;
#4488 = CARTESIAN_POINT ( 'NONE',  ( -9.989344678689363377, 9.809645194533960222, 7.995959430373565269 ) ) ;
#4489 = CARTESIAN_POINT ( 'NONE',  ( 4.766900247265192903, 9.355568503977902850, 18.60000000000000497 ) ) ;
#4490 = CARTESIAN_POINT ( 'NONE',  ( 16.30827793483735633, -1.837501619626142890, 8.357142857142855874 ) ) ;
#4491 = CARTESIAN_POINT ( 'NONE',  ( 16.30827793483735633, -1.837501619626142890, 8.357142857142855874 ) ) ;
#4492 = APPLICATION_PROTOCOL_DEFINITION ( 'draft international standard', 'automotive_design', 1998, #2562 ) ;
#4493 = CARTESIAN_POINT ( 'NONE',  ( -13.21436662431716869, 4.623906867372262752, 29.57142857142857650 ) ) ;
#4494 = AXIS2_PLACEMENT_3D ( 'NONE', #1579, #4577, #6161 ) ;
#4495 = CLOSED_SHELL ( 'NONE', ( #4374, #1806, #6248, #9894 ) ) ;
#4496 = AXIS2_PLACEMENT_3D ( 'NONE', #9182, #3584, #6110 ) ;
#4497 = EDGE_LOOP ( 'NONE', ( #9724, #5205, #1116, #1808 ) ) ;
#4498 = CARTESIAN_POINT ( 'NONE',  ( 4.619798703721856192, 13.59724543428036725, 45.06738800180215065 ) ) ;
#4499 = ORIENTED_EDGE ( 'NONE', *, *, #8056, .F. ) ;
#4500 = CARTESIAN_POINT ( 'NONE',  ( 5.986002070941135678, -13.58603705635637304, -1.270000000000007123 ) ) ;
#4501 = CARTESIAN_POINT ( 'NONE',  ( 11.40355824106246985, -11.22385875690704538, 28.99595943037357060 ) ) ;
#4502 = CARTESIAN_POINT ( 'NONE',  ( 11.31370849898482334, -11.31370849898469366, 3.000000000000002665 ) ) ;
#4503 = CARTESIAN_POINT ( 'NONE',  ( 10.89658364409024749, 1.776620879821585897, 17.04886208192142760 ) ) ;
#4504 = CARTESIAN_POINT ( 'NONE',  ( -4.619798703721853528, -13.59724543428036725, 48.06738800180213644 ) ) ;
#4505 = CARTESIAN_POINT ( 'NONE',  ( 9.837026868206066865, -5.012215536711391195, 10.35000000000002274 ) ) ;
#4506 = CARTESIAN_POINT ( 'NONE',  ( 7.842167650704563897, 7.771249796623195039, 14.75113791807856956 ) ) ;
#4507 = CARTESIAN_POINT ( 'NONE',  ( -55.00000000000002132, 2.079464148194913206E-15, -18.00000000000000000 ) ) ;
#4508 = CARTESIAN_POINT ( 'NONE',  ( 1.693770420379222319, 13.89774397934251837, 34.86118342676929416 ) ) ;
#4509 = VECTOR ( 'NONE', #586, 1000.000000000000000 ) ;
#4510 = CARTESIAN_POINT ( 'NONE',  ( -4.766900247265192014, -9.355568503977876205, 14.10000000000000142 ) ) ;
#4511 = CARTESIAN_POINT ( 'NONE',  ( 9.989344678689365153, -9.809645194533958446, 4.995959430373563492 ) ) ;
#4512 = CARTESIAN_POINT ( 'NONE',  ( -10.90442828429184274, -1.727091770866655773, 8.549999999999963407 ) ) ;
#4513 = FACE_BOUND ( 'NONE', #6385, .T. ) ;
#4514 = CARTESIAN_POINT ( 'NONE',  ( 13.51115193377584589, 4.865839792409294873, 15.92453085894499409 ) ) ;
#4515 = CARTESIAN_POINT ( 'NONE',  ( -6.683790977649319842, 6.751237864895101026, 17.00113791807859442 ) ) ;
#4516 = CARTESIAN_POINT ( 'NONE',  ( -1.612135949262737844, -9.858066664633893694, 3.951137918078560851 ) ) ;
#4517 = DIRECTION ( 'NONE',  ( -1.000000000000000000, 0.000000000000000000, 0.000000000000000000 ) ) ;
#4518 = CARTESIAN_POINT ( 'NONE',  ( -13.21436662431716869, 4.623906867372262752, 41.57142857142856940 ) ) ;
#4519 = CARTESIAN_POINT ( 'NONE',  ( -14.26974319298268767, 1.607813917172874918, 47.35714285714286120 ) ) ;
#4520 = ORIENTED_EDGE ( 'NONE', *, *, #9479, .F. ) ;
#4521 = CARTESIAN_POINT ( 'NONE',  ( 13.47998361472151529, 8.620103694222146729, 9.710245144659278793 ) ) ;
#4522 = CARTESIAN_POINT ( 'NONE',  ( -6.162860009432963970, 14.69216993800150739, -4.192871190346624312E-15 ) ) ;
#4523 = ADVANCED_FACE ( 'NONE', ( #6537 ), #9133, .T. ) ;
#4524 = CARTESIAN_POINT ( 'NONE',  ( -15.10213328493390961, 5.284464991282586510, 35.57142857142857650 ) ) ;
#4525 = LINE ( 'NONE', #2143, #7149 ) ;
#4526 = FILL_AREA_STYLE_COLOUR ( '', #851 ) ;
#4527 = CARTESIAN_POINT ( 'NONE',  ( 7.424621202458790314, -7.424621202458697944, 1.500000000000001332 ) ) ;
#4528 = CARTESIAN_POINT ( 'NONE',  ( -1.486127417882243895, 9.383039235653825472, 9.299999999999975842 ) ) ;
#4529 = CARTESIAN_POINT ( 'NONE',  ( -7.027753727702738651, -7.098671581784262941, 15.24886208192144110 ) ) ;
#4530 = EDGE_CURVE ( 'NONE', #3374, #8249, #4418, .T. ) ;
#4531 = DIRECTION ( 'NONE',  ( 0.000000000000000000, 6.338944243255235518E-49, -1.000000000000000000 ) ) ;
#4532 = CARTESIAN_POINT ( 'NONE',  ( 11.60466159355862104, 11.60466159355875071, 43.50000000000000711 ) ) ;
#4533 =( NAMED_UNIT ( * ) SI_UNIT ( $, .STERADIAN. ) SOLID_ANGLE_UNIT ( ) );
#4534 = CIRCLE ( 'NONE', #4352, 8.500000000000000000 ) ;
#4535 = CARTESIAN_POINT ( 'NONE',  ( -15.53355953199861794, -5.297344310588530725, 20.93261199819787066 ) ) ;
#4536 = CARTESIAN_POINT ( 'NONE',  ( 7.448449071214646722, 11.85413878919601594, 31.28571428571428470 ) ) ;
#4537 = CARTESIAN_POINT ( 'NONE',  ( 16.30827793483735633, -1.837501619626142890, 14.35714285714285587 ) ) ;
#4538 = CARTESIAN_POINT ( 'NONE',  ( -16.30827793483735988, 1.837501619626141780, 47.35714285714286120 ) ) ;
#4539 = ORIENTED_EDGE ( 'NONE', *, *, #9349, .F. ) ;
#4540 = CARTESIAN_POINT ( 'NONE',  ( -7.424621202458789426, 7.424621202458723701, 15.00000000000001421 ) ) ;
#4541 = DIRECTION ( 'NONE',  ( 0.000000000000000000, -1.000000000000000000, 0.000000000000000000 ) ) ;
#4542 = CARTESIAN_POINT ( 'NONE',  ( -8.731428362939187338, 13.89598863503036164, 48.21428571428571530 ) ) ;
#4543 = CARTESIAN_POINT ( 'NONE',  ( 0.000000000000000000, 0.000000000000000000, 0.000000000000000000 ) ) ;
#4544 = EDGE_CURVE ( 'NONE', #7640, #7109, #1359, .T. ) ;
#4545 = CARTESIAN_POINT ( 'NONE',  ( 5.012215536711511987, -9.837026868205999364, 13.65000000000003233 ) ) ;
#4546 = CARTESIAN_POINT ( 'NONE',  ( -15.49051278174638036, -5.420364854932175902, 4.928571428571430602 ) ) ;
#4547 = CARTESIAN_POINT ( 'NONE',  ( -8.621071003556675549, 13.96533075980314642, 46.21832628391216247 ) ) ;
#4548 = DIRECTION ( 'NONE',  ( 0.9745501978280481925, -0.2241693821941616593, 5.967398901892713276E-17 ) ) ;
#4549 = EDGE_CURVE ( 'NONE', #1309, #9252, #7106, .T. ) ;
#4550 = SHAPE_REPRESENTATION ( 'round tube', ( #3995 ), #6945 ) ;
#4551 = CARTESIAN_POINT ( 'NONE',  ( 11.85413878919593422, 7.448449071214774619, 19.71428571428571175 ) ) ;
#4552 = CARTESIAN_POINT ( 'NONE',  ( 4.743843029824831525, -13.17239914596749095, 47.42453085894499765 ) ) ;
#4553 = ORIENTED_EDGE ( 'NONE', *, *, #9373, .T. ) ;
#4554 = DIRECTION ( 'NONE',  ( 0.000000000000000000, -6.338944243255235518E-49, 1.000000000000000000 ) ) ;
#4555 = CARTESIAN_POINT ( 'NONE',  ( 1.967016585148662289, -16.29368510291087091, 17.63881657323070939 ) ) ;
#4556 = CARTESIAN_POINT ( 'NONE',  ( -0.3021515714675195863, 13.99673906407701729, 48.73000000000003951 ) ) ;
#4557 = CARTESIAN_POINT ( 'NONE',  ( 8.442910196168311288, 4.355403765523576887, 7.898862081921404155 ) ) ;
#4558 = CARTESIAN_POINT ( 'NONE',  ( 11.51250119794888249, 11.69682198916847682, 27.49595943037356705 ) ) ;
#4559 = CARTESIAN_POINT ( 'NONE',  ( -9.837026868206066865, 5.012215536711416064, 5.849999999999989875 ) ) ;
#4560 = CARTESIAN_POINT ( 'NONE',  ( 1.595456901104624459, -10.37818827243064668, 9.801137918078557831 ) ) ;
#4561 = CARTESIAN_POINT ( 'NONE',  ( -1.925929944387235853E-31, -1.018491042385001544, -1.270000000000007123 ) ) ;
#4562 = CARTESIAN_POINT ( 'NONE',  ( 7.556039541191335474, 11.78653521626503320, 29.28975485534071765 ) ) ;
#4563 = CARTESIAN_POINT ( 'NONE',  ( 15.88516839912898071, 1.917699372586004092, 46.13881657323070584 ) ) ;
#4564 = CARTESIAN_POINT ( 'NONE',  ( -7.424621202458789426, 7.424621202458720148, 3.000000000000002665 ) ) ;
#4565 = CARTESIAN_POINT ( 'NONE',  ( -15.89939535829186923, -1.791431617653016062, 29.14285714285714235 ) ) ;
#4566 = DIRECTION ( 'NONE',  ( 0.000000000000000000, 0.000000000000000000, -1.000000000000000000 ) ) ;
#4567 = CARTESIAN_POINT ( 'NONE',  ( 12.22833218042443271, -7.529642458189144349, 10.78167371608784819 ) ) ;
#4568 = CARTESIAN_POINT ( 'NONE',  ( 1.439022436064387511, -9.390499931835517344, 12.80113791807860224 ) ) ;
#4569 = CARTESIAN_POINT ( 'NONE',  ( 8.877401133907127928, -4.579542530753017537, 9.351137918078563871 ) ) ;
#4570 = CARTESIAN_POINT ( 'NONE',  ( 61.99999999999997158, 0.000000000000000000, 0.000000000000000000 ) ) ;
#4571 = CARTESIAN_POINT ( 'NONE',  ( -13.91197093850538380, -1.567502665446387278, 41.14285714285714590 ) ) ;
#4572 = CARTESIAN_POINT ( 'NONE',  ( -7.448449071214644945, -11.85413878919601771, 46.28571428571429180 ) ) ;
#4573 = EDGE_LOOP ( 'NONE', ( #7823, #3451, #5167, #2705 ) ) ;
#4575 = DIRECTION ( 'NONE',  ( 0.000000000000000000, 0.000000000000000000, 1.000000000000000000 ) ) ;
#4574 = CIRCLE ( 'NONE', #283, 0.9906000000000003691 ) ;
#4576 = CARTESIAN_POINT ( 'NONE',  ( 8.512513224245308763, 13.54758718765259040, 25.28571428571428470 ) ) ;
#4577 = DIRECTION ( 'NONE',  ( 0.000000000000000000, -6.338944243255235518E-49, 1.000000000000000000 ) ) ;
#4578 = LINE ( 'NONE', #8343, #4801 ) ;
#4579 = CARTESIAN_POINT ( 'NONE',  ( -1.486127417882243895, 9.383039235653816590, 3.299999999999969624 ) ) ;
#4580 = CARTESIAN_POINT ( 'NONE',  ( -8.922933199037192509, 4.490180821391425603, 15.84886208192146739 ) ) ;
#4581 = DIRECTION ( 'NONE',  ( 0.000000000000000000, -1.000000000000000000, 9.714451465470119729E-16 ) ) ;
#4582 = CARTESIAN_POINT ( 'NONE',  ( 13.61519076058348254, 8.404922754268771001, 17.71832628391214826 ) ) ;
#4583 = CARTESIAN_POINT ( 'NONE',  ( 8.512513224245308763, 13.54758718765259040, 37.28571428571429180 ) ) ;
#4584 = AXIS2_PLACEMENT_3D ( 'NONE', #6285, #4129, #3203 ) ;
#4585 = SHAPE_REPRESENTATION_RELATIONSHIP ( 'NONE' , 'NONE' ,  #5586, #8958 ) ;
#4586 = CARTESIAN_POINT ( 'NONE',  ( 15.91362231745475597, 1.665163862720026255, 18.14689771248357530 ) ) ;
#4587 = VERTEX_POINT ( 'NONE', #3636 ) ;
#4588 = DIRECTION ( 'NONE',  ( -4.755747939841216568E-17, 1.000000000000000000, 0.000000000000000000 ) ) ;
#4589 = ORIENTED_EDGE ( 'NONE', *, *, #9652, .F. ) ;
#4590 = CARTESIAN_POINT ( 'NONE',  ( -4.766900247265192014, -9.355568503977867323, 11.09999999999999787 ) ) ;
#4591 = EDGE_LOOP ( 'NONE', ( #2957, #3408, #5369, #7462 ) ) ;
#4592 = CARTESIAN_POINT ( 'NONE',  ( 8.731428362939189114, -13.89598863503035986, 45.21428571428572951 ) ) ;
#4593 = CARTESIAN_POINT ( 'NONE',  ( -9.859792900771106261, 4.967534682030611215, 12.84886208192143009 ) ) ;
#4594 = CARTESIAN_POINT ( 'NONE',  ( -5.164528828830334817, 15.14410076328347543, 46.43261199819787066 ) ) ;
#4595 = ITEM_DEFINED_TRANSFORMATION ( 'NONE', 'NONE', #7233,  #3995 ) ;
#4596 = CARTESIAN_POINT ( 'NONE',  ( 13.55419868402807992, 4.742819248065649695, 25.92857142857143060 ) ) ;
#4597 = CARTESIAN_POINT ( 'NONE',  ( -1.562606840307830591, -9.865911304835481843, 10.95000000000000284 ) ) ;
#4598 = CARTESIAN_POINT ( 'NONE',  ( 13.25633410266679313, -4.503970704919842305, 34.56738800180213644 ) ) ;
#4599 = FACE_OUTER_BOUND ( 'NONE', #9240, .T. ) ;
#4600 = B_SPLINE_CURVE_WITH_KNOTS ( 'NONE', 3,
 ( #9378, #7037, #8650, #1521, #6252, #5492, #1573, #10041, #8440, #6099, #7819, #8545, #2340, #3009, #1364, #1468, #7865, #9431, #2135, #9278, #699, #2900, #792, #7724, #5435, #2292, #5279, #6820, #2192, #6044 ),
 .UNSPECIFIED., .F., .F.,
 ( 4, 2, 2, 2, 2, 2, 2, 2, 2, 2, 2, 2, 2, 2, 4 ),
 ( 0.006733453442732789153, 0.007574925429288498560, 0.007995661422566354565, 0.008416397415844208835, 0.008837133409122063105, 0.009257869402399917375, 0.009678605395677773379, 0.01009934138895562765, 0.01052007738223348365, 0.01094081337551133792, 0.01136154936878919219, 0.01178228536206704646, 0.01262375734862281572, 0.01304449334190071683, 0.01346522933517861620 ),
 .UNSPECIFIED. ) ;
#4601 = ORIENTED_EDGE ( 'NONE', *, *, #6775, .T. ) ;
#4602 = CARTESIAN_POINT ( 'NONE',  ( -170.0000000000000284, 12.99999999999999289, 0.000000000000000000 ) ) ;
#4603 = CARTESIAN_POINT ( 'NONE',  ( 11.51250119794888249, 11.69682198916847682, 21.49595943037356705 ) ) ;
#4604 = CARTESIAN_POINT ( 'NONE',  ( -13.89598863503045933, 8.731428362939027465, 5.785714285714282923 ) ) ;
#4605 = CARTESIAN_POINT ( 'NONE',  ( -1.513077731352923339, -9.873755945037078874, 8.948862081921467038 ) ) ;
#4606 = CARTESIAN_POINT ( 'NONE',  ( 5.297344310588354865, 15.53355953199867301, 27.06738800180213644 ) ) ;
#4607 = CARTESIAN_POINT ( 'NONE',  ( -156.0000000000000284, -6.938893903907228378E-15, 0.000000000000000000 ) ) ;
#4608 = CARTESIAN_POINT ( 'NONE',  ( 7.842167650704563897, 7.771249796623202144, 11.75113791807857666 ) ) ;
#4609 = DIRECTION ( 'NONE',  ( 1.000000000000000000, 0.000000000000000000, 0.000000000000000000 ) ) ;
#4610 = CARTESIAN_POINT ( 'NONE',  ( -10.24623928997352351, -10.06191849875416899, 44.50404056962644006 ) ) ;
#4611 = CARTESIAN_POINT ( 'NONE',  ( -4.619798703721853528, -13.59724543428036725, 6.067388001802139996 ) ) ;
#4612 = CARTESIAN_POINT ( 'NONE',  ( -158.0000000000000284, -13.00000000000000711, 1.592040838891559095E-15 ) ) ;
#4613 = DIRECTION ( 'NONE',  ( 1.000000000000000000, -4.575525868300071581E-16, -0.000000000000000000 ) ) ;
#4614 = CARTESIAN_POINT ( 'NONE',  ( 4.743843029824831525, -13.17239914596749095, 23.42453085894499409 ) ) ;
#4615 = CARTESIAN_POINT ( 'NONE',  ( -10.36326688006724162, 1.689666864740235308, 7.701137918078540423 ) ) ;
#4616 = CARTESIAN_POINT ( 'NONE',  ( 6.683790977649321619, -6.751237864895077045, 0.5011379180785839882 ) ) ;
#4617 = CARTESIAN_POINT ( 'NONE',  ( -170.0000000000000284, -8.084771497730068080E-15, 0.000000000000000000 ) ) ;
#4618 = CARTESIAN_POINT ( 'NONE',  ( 5.543385399275644332, 15.44746603149420494, 41.07546914105501656 ) ) ;
#4619 = CARTESIAN_POINT ( 'NONE',  ( -13.91197093850538380, -1.567502665446387278, 47.14285714285714590 ) ) ;
#4620 = CARTESIAN_POINT ( 'NONE',  ( 1.607813917173038121, -14.26974319298267346, 45.64285714285716011 ) ) ;
#4621 = ORIENTED_EDGE ( 'NONE', *, *, #7934, .F. ) ;
#4622 = CARTESIAN_POINT ( 'NONE',  ( 11.40355824106246985, -11.22385875690704538, 10.99595943037356882 ) ) ;
#4623 = DIRECTION ( 'NONE',  ( 0.000000000000000000, -6.338944243255235518E-49, 1.000000000000000000 ) ) ;
#4624 = CARTESIAN_POINT ( 'NONE',  ( -16.30827793483735988, 1.837501619626141780, 47.35714285714286120 ) ) ;
#4625 = CARTESIAN_POINT ( 'NONE',  ( 8.560346291714190440E-16, -18.00000000000000355, 2.204364238465235822E-15 ) ) ;
#4626 = DIRECTION ( 'NONE',  ( 0.000000000000000000, 6.938893903907221444E-18, 1.000000000000000000 ) ) ;
#4627 = CIRCLE ( 'NONE', #832, 16.00000000000000000 ) ;
#4628 = CARTESIAN_POINT ( 'NONE',  ( -4.534861676072319270, 8.900167166472117586, 6.149999999999980815 ) ) ;
#4629 = CARTESIAN_POINT ( 'NONE',  ( 8.922933199037192509, -4.490180821391404287, 20.34886208192140700 ) ) ;
#4630 = CARTESIAN_POINT ( 'NONE',  ( -108.0000000000000284, 0.000000000000000000, 0.000000000000000000 ) ) ;
#4631 = CARTESIAN_POINT ( 'NONE',  ( 5.420364854932001819, 15.49051278174644430, 43.07142857142858361 ) ) ;
#4632 =( NAMED_UNIT ( * ) SI_UNIT ( $, .STERADIAN. ) SOLID_ANGLE_UNIT ( ) );
#4633 = CARTESIAN_POINT ( 'NONE',  ( -15.06016580658428694, 5.404401153735006957, 15.57546914105500413 ) ) ;
#4634 = VECTOR ( 'NONE', #9964, 1000.000000000000000 ) ;
#4635 = AXIS2_PLACEMENT_3D ( 'NONE', #9486, #948, #2591 ) ;
#4636 = CARTESIAN_POINT ( 'NONE',  ( -16.30827793483735988, 1.837501619626141780, 23.35714285714286476 ) ) ;
#4637 = CARTESIAN_POINT ( 'NONE',  ( -88.00000000000002842, 1.592040838891559095E-15, -13.00000000000000000 ) ) ;
#4638 = CARTESIAN_POINT ( 'NONE',  ( 9.355568503977840678, 4.766900247265305701, 15.90000000000002522 ) ) ;
#4639 = CARTESIAN_POINT ( 'NONE',  ( 16.30827793483735633, -1.837501619626142890, 38.35714285714286831 ) ) ;
#4640 = AXIS2_PLACEMENT_3D ( 'NONE', #810, #5456, #4588 ) ;
#4641 = DIRECTION ( 'NONE',  ( 1.000000000000000000, 0.000000000000000000, 0.000000000000000000 ) ) ;
#4642 = AXIS2_PLACEMENT_3D ( 'NONE', #5903, #9135, #4168 ) ;
#4643 = CIRCLE ( 'NONE', #7281, 16.99999999999997868 ) ;
#4644 = CARTESIAN_POINT ( 'NONE',  ( 4.724406229267374968, 9.377220287599064008, 7.598862081921438971 ) ) ;
#4645 = CARTESIAN_POINT ( 'NONE',  ( -1.707986654103994528, 16.32287076676380266, 46.64689771248358596 ) ) ;
#4646 = ITEM_DEFINED_TRANSFORMATION ( 'NONE', 'NONE', #5896,  #3995 ) ;
#4647 = CARTESIAN_POINT ( 'NONE',  ( -14.26974319298268767, 1.607813917172874696, 29.35714285714286120 ) ) ;
#4648 = AXIS2_PLACEMENT_3D ( 'NONE', #1624, #4675, #17 ) ;
#4649 = CARTESIAN_POINT ( 'NONE',  ( -8.464561979789474222, -4.312909747525728754, 5.400000000000016342 ) ) ;
#4650 = EDGE_LOOP ( 'NONE', ( #388, #4379, #5159, #4762 ) ) ;
#4651 = CARTESIAN_POINT ( 'NONE',  ( 1.441234910513245149, 13.92619789766829008, 38.85310228751641404 ) ) ;
#4652 = ORIENTED_EDGE ( 'NONE', *, *, #6228, .F. ) ;
#4653 = FACE_OUTER_BOUND ( 'NONE', #1800, .T. ) ;
#4654 = CARTESIAN_POINT ( 'NONE',  ( -15.44746603149413922, -5.543385399275820191, 24.92453085894499765 ) ) ;
#4655 = CARTESIAN_POINT ( 'NONE',  ( 8.731428362939189114, -13.89598863503035986, 9.214285714285717077 ) ) ;
#4656 = CARTESIAN_POINT ( 'NONE',  ( 11.40355824106246985, -11.22385875690704538, 22.99595943037356705 ) ) ;
#4657 = CYLINDRICAL_SURFACE ( 'NONE', #3623, 8.000000000000000000 ) ;
#4658 = CARTESIAN_POINT ( 'NONE',  ( -4.967534682030703586, 9.859792900771061852, 17.15113791807853616 ) ) ;
#4659 = EDGE_CURVE ( 'NONE', #7745, #8337, #1855, .T. ) ;
#4660 = FACE_OUTER_BOUND ( 'NONE', #10025, .T. ) ;
#4661 = ORIENTED_EDGE ( 'NONE', *, *, #1909, .F. ) ;
#4662 = CARTESIAN_POINT ( 'NONE',  ( 7.340858601237956194, 11.92174236212700045, 9.281673716087846415 ) ) ;
#4663 = CARTESIAN_POINT ( 'NONE',  ( 1.642561882922480621, -10.37072757624891750, 7.800000000000029132 ) ) ;
#4664 = DIRECTION ( 'NONE',  ( -1.000000000000000000, 0.000000000000000000, 0.000000000000000000 ) ) ;
#4665 = CARTESIAN_POINT ( 'NONE',  ( -10.06191849875405531, -10.24623928997363542, 30.49595943037356349 ) ) ;
#4666 = CARTESIAN_POINT ( 'NONE',  ( 1.595456901104624459, -10.37818827243064668, 9.801137918078557831 ) ) ;
#4667 = CARTESIAN_POINT ( 'NONE',  ( -4.355403765523468529, -8.442910196168346815, 1.101137918078559208 ) ) ;
#4668 = CARTESIAN_POINT ( 'NONE',  ( -158.0000000000000284, -6.938893903907228378E-15, 0.000000000000000000 ) ) ;
#4669 = CARTESIAN_POINT ( 'NONE',  ( -1.707986654103994528, 16.32287076676380266, 46.64689771248358596 ) ) ;
#4670 = CARTESIAN_POINT ( 'NONE',  ( -4.503970704919988854, 13.25633410266674517, 4.432611998197859116 ) ) ;
#4671 = PRODUCT_DEFINITION ( 'UNKNOWN', '', #970, #6776 ) ;
#4672 = CARTESIAN_POINT ( 'NONE',  ( -7.529642458189277576, 12.22833218042435455, 4.218326283912150032 ) ) ;
#4673 = ORIENTED_EDGE ( 'NONE', *, *, #2093, .F. ) ;
#4674 = CARTESIAN_POINT ( 'NONE',  ( -13.47998361472151174, -8.620103694222146729, 12.71024514465927879 ) ) ;
#4675 = DIRECTION ( 'NONE',  ( -1.000000000000000000, -0.000000000000000000, -0.000000000000000000 ) ) ;
#4676 = CARTESIAN_POINT ( 'NONE',  ( 15.89939535829187278, 1.791431617653015174, 38.14285714285714590 ) ) ;
#4677 = CYLINDRICAL_SURFACE ( 'NONE', #4309, 3.632199999999998763 ) ;
#4678 = CARTESIAN_POINT ( 'NONE',  ( 4.995402070941135086, -13.58603705635637304, 0.000000000000000000 ) ) ;
#4679 = APPLICATION_CONTEXT ( 'automotive_design' ) ;
#4680 = CARTESIAN_POINT ( 'NONE',  ( 4.534861676072320158, -8.900167166472098046, 13.65000000000003233 ) ) ;
#4681 = CARTESIAN_POINT ( 'NONE',  ( -1.513077731352923339, -9.873755945037078874, 17.94886208192144395 ) ) ;
#4682 = CARTESIAN_POINT ( 'NONE',  ( 0.000000000000000000, 0.000000000000000000, 0.000000000000000000 ) ) ;
#4683 = CARTESIAN_POINT ( 'NONE',  ( -8.900167166472160218, 4.534861676072232228, 2.849999999999968114 ) ) ;
#4684 = FILL_AREA_STYLE_COLOUR ( '', #7288 ) ;
#4685 = CARTESIAN_POINT ( 'NONE',  ( -11.22385875690717327, 11.40355824106234550, 22.00404056962643651 ) ) ;
#4686 = CARTESIAN_POINT ( 'NONE',  ( 5.420364854932001819, 15.49051278174644430, 13.07142857142857295 ) ) ;
#4687 = CARTESIAN_POINT ( 'NONE',  ( 2.000000000000001776, -1.773042676681352292, -1.110223024625156540E-13 ) ) ;
#4688 = CARTESIAN_POINT ( 'NONE',  ( 8.731428362939190890, -13.89598863503036164, 3.214285714285716633 ) ) ;
#4689 = CARTESIAN_POINT ( 'NONE',  ( 11.31370849898482334, -11.31370849898469366, 39.00000000000000000 ) ) ;
#4690 = SURFACE_STYLE_USAGE ( .BOTH. , #2979 ) ;
#4691 = EDGE_CURVE ( 'NONE', #9817, #2212, #1213, .T. ) ;
#4692 = CIRCLE ( 'NONE', #234, 1.000000000000000000 ) ;
#4693 = CARTESIAN_POINT ( 'NONE',  ( -4.724406229267374968, -9.377220287599040915, 9.098862081921437195 ) ) ;
#4694 = CARTESIAN_POINT ( 'NONE',  ( -16.30827793483735988, 1.837501619626141780, 5.357142857142856762 ) ) ;
#4695 = ITEM_DEFINED_TRANSFORMATION ( 'NONE', 'NONE', #5576,  #3995 ) ;
#4696 = CARTESIAN_POINT ( 'NONE',  ( 14.26974319298268767, -1.607813917172876472, 32.35714285714286120 ) ) ;
#4697 = CARTESIAN_POINT ( 'NONE',  ( 12.08964793087886314, -7.750357176954162597, 30.78975485534071765 ) ) ;
#4698 = CARTESIAN_POINT ( 'NONE',  ( 8.900167166472158442, -4.534861676072210912, 7.350000000000000533 ) ) ;
#4699 = CARTESIAN_POINT ( 'NONE',  ( -10.37072757624895836, 1.642561882922380923, 17.69999999999999218 ) ) ;
#4700 = ORIENTED_EDGE ( 'NONE', *, *, #5122, .F. ) ;
#4701 = CARTESIAN_POINT ( 'NONE',  ( -7.639999817571787588, 12.15899005565156266, 0.2142857142857168273 ) ) ;
#4702 = DIRECTION ( 'NONE',  ( -1.000000000000000000, 1.842239752758738928E-31, 1.840628461782073167E-32 ) ) ;
#4703 = CARTESIAN_POINT ( 'NONE',  ( -15.14410076328353227, 5.164528828830164287, 19.56738800180213644 ) ) ;
#4704 = CARTESIAN_POINT ( 'NONE',  ( 15.10213328493390783, -5.284464991282587398, 2.571428571428571619 ) ) ;
#4705 = CARTESIAN_POINT ( 'NONE',  ( -8.404922754268618235, -13.61519076058357491, 30.28167371608785530 ) ) ;
#4706 = CARTESIAN_POINT ( 'NONE',  ( 9.837026868206066865, -5.012215536711392083, 1.350000000000015188 ) ) ;
#4707 = CARTESIAN_POINT ( 'NONE',  ( -1.727091770866549414, -10.90442828429184630, 1.949999999999996181 ) ) ;
#4708 = CARTESIAN_POINT ( 'NONE',  ( -7.448449071214644945, -11.85413878919601771, 4.285714285714288252 ) ) ;
#4709 =( NAMED_UNIT ( * ) SI_UNIT ( $, .STERADIAN. ) SOLID_ANGLE_UNIT ( ) );
#4710 = VERTEX_POINT ( 'NONE', #9954 ) ;
#4711 = CARTESIAN_POINT ( 'NONE',  ( -5.404401153735176599, 15.06016580658422477, 50.42453085894499765 ) ) ;
#4712 = ADVANCED_FACE ( 'NONE', ( #7330 ), #5236, .F. ) ;
#4713 = CARTESIAN_POINT ( 'NONE',  ( -1.727091770866549414, -10.90442828429185695, 4.950000000000017941 ) ) ;
#4714 = CARTESIAN_POINT ( 'NONE',  ( -11.60466159355861926, -11.60466159355875249, 10.50000000000000533 ) ) ;
#4715 = DIRECTION ( 'NONE',  ( 0.000000000000000000, -1.000000000000000000, 0.000000000000000000 ) ) ;
#4716 = CARTESIAN_POINT ( 'NONE',  ( -9.989344678689363377, 9.809645194533960222, 31.99595943037357060 ) ) ;
#4717 = CARTESIAN_POINT ( 'NONE',  ( -4.809394265263009061, -9.333916720356723928, 4.101137918078561206 ) ) ;
#4718 = CARTESIAN_POINT ( 'NONE',  ( 6.683790977649321619, -6.751237864895076157, 18.50113791807859087 ) ) ;
#4719 = EDGE_CURVE ( 'NONE', #4150, #8824, #868, .T. ) ;
#4720 = DIRECTION ( 'NONE',  ( -1.000000000000000000, 0.000000000000000000, 0.000000000000000000 ) ) ;
#4721 = CARTESIAN_POINT ( 'NONE',  ( 7.556039541191335474, 11.78653521626503320, 11.28975485534071943 ) ) ;
#4722 = CARTESIAN_POINT ( 'NONE',  ( -1.693770420379220099, -13.89774397934251837, 13.86118342676929416 ) ) ;
#4723 = VERTEX_POINT ( 'NONE', #2088 ) ;
#4724 = CARTESIAN_POINT ( 'NONE',  ( -5.297344310588352201, -15.53355953199867301, 6.067388001802139996 ) ) ;
#4725 = DIRECTION ( 'NONE',  ( 1.000000000000000000, 0.000000000000000000, 0.000000000000000000 ) ) ;
#4726 = CARTESIAN_POINT ( 'NONE',  ( -15.49051278174638036, -5.420364854932175902, 40.92857142857145192 ) ) ;
#4727 = FACE_OUTER_BOUND ( 'NONE', #6222, .T. ) ;
#4728 = EDGE_CURVE ( 'NONE', #5215, #8337, #4525, .T. ) ;
#4729 = CARTESIAN_POINT ( 'NONE',  ( -1.486127417882243895, 9.383039235653816590, 12.29999999999997762 ) ) ;
#4730 = CARTESIAN_POINT ( 'NONE',  ( 1.513077731352925115, 9.873755945037100190, 13.44886208192141197 ) ) ;
#4731 = DIRECTION ( 'NONE',  ( -1.000000000000000000, -1.387778780781445676E-16, -0.000000000000000000 ) ) ;
#4732 = CARTESIAN_POINT ( 'NONE',  ( -15.53355953199861794, -5.297344310588530725, 32.93261199819787777 ) ) ;
#4733 = CARTESIAN_POINT ( 'NONE',  ( -7.063212654743467489, -7.063212654743535879, 2.249999999999986677 ) ) ;
#4734 = CARTESIAN_POINT ( 'NONE',  ( -8.620103694221995738, -13.47998361472161299, 32.28975485534072476 ) ) ;
#4735 = CARTESIAN_POINT ( 'NONE',  ( -16.30827793483735988, 1.837501619626141780, 17.35714285714286476 ) ) ;
#4736 = DIRECTION ( 'NONE',  ( 0.000000000000000000, -1.000000000000000000, 0.000000000000000000 ) ) ;
#4737 = CARTESIAN_POINT ( 'NONE',  ( 4.000000000000003553, 2.866884953888006423E-33, 3.500000000000000000 ) ) ;
#4738 =( NAMED_UNIT ( * ) SI_UNIT ( $, .STERADIAN. ) SOLID_ANGLE_UNIT ( ) );
#4739 = SURFACE_SIDE_STYLE ('',( #4940 ) ) ;
#4740 = CARTESIAN_POINT ( 'NONE',  ( 0.000000000000000000, 0.000000000000000000, 0.000000000000000000 ) ) ;
#4741 = AXIS2_PLACEMENT_3D ( 'NONE', #7246, #4199, #4051 ) ;
#4742 = PRODUCT_DEFINITION_CONTEXT ( 'detailed design', #7509, 'design' ) ;
#4743 = CARTESIAN_POINT ( 'NONE',  ( -10.37818827243067688, 1.595456901104524761, 6.698862081921455491 ) ) ;
#4744 = CARTESIAN_POINT ( 'NONE',  ( 4.503970704919991519, -13.25633410266674517, 43.43261199819787066 ) ) ;
#4745 = CARTESIAN_POINT ( 'NONE',  ( -8.512513224245306986, -13.54758718765259218, 16.28571428571428470 ) ) ;
#4746 = CONTEXT_DEPENDENT_SHAPE_REPRESENTATION ( #8165, #2100 ) ;
#4747 = CARTESIAN_POINT ( 'NONE',  ( -1.567502665446231180, -13.91197093850540334, 39.85714285714286120 ) ) ;
#4748 = CARTESIAN_POINT ( 'NONE',  ( 11.92174236212692229, 7.340858601238088532, 35.71832628391214115 ) ) ;
#4749 = CARTESIAN_POINT ( 'NONE',  ( -8.464561979789474222, -4.312909747525729642, 14.39999999999996838 ) ) ;
#4750 = CARTESIAN_POINT ( 'NONE',  ( 5.012215536711511987, -9.837026868205999364, 16.64999999999999858 ) ) ;
#4751 = ORIENTED_EDGE ( 'NONE', *, *, #2699, .T. ) ;
#4752 = CARTESIAN_POINT ( 'NONE',  ( 13.55419868402807992, 4.742819248065648807, 1.928571428571430380 ) ) ;
#4753 = ORIENTED_EDGE ( 'NONE', *, *, #2720, .T. ) ;
#4754 = FACE_OUTER_BOUND ( 'NONE', #2629, .T. ) ;
#4755 = CARTESIAN_POINT ( 'NONE',  ( -15.88516839912898071, -1.917699372586004980, 31.13881657323070939 ) ) ;
#4756 = STYLED_ITEM ( 'NONE', ( #9573 ), #9458 ) ;
#4757 = CARTESIAN_POINT ( 'NONE',  ( -8.731428362939187338, 13.89598863503036164, 18.21428571428572241 ) ) ;
#4758 = CARTESIAN_POINT ( 'NONE',  ( 8.404922754268618235, 13.61519076058357491, 21.28167371608785530 ) ) ;
#4759 = LINE ( 'NONE', #6140, #6737 ) ;
#4760 = CARTESIAN_POINT ( 'NONE',  ( -9.837026868206066865, 5.012215536711416064, 5.849999999999989875 ) ) ;
#4761 = DIRECTION ( 'NONE',  ( -0.000000000000000000, 1.000000000000000000, 1.224646799147353207E-16 ) ) ;
#4762 = ORIENTED_EDGE ( 'NONE', *, *, #882, .F. ) ;
#4763 = CARTESIAN_POINT ( 'NONE',  ( -9.837026868206070418, 5.012215536711412511, 14.84999999999999609 ) ) ;
#4764 = FACE_OUTER_BOUND ( 'NONE', #3716, .T. ) ;
#4765 = CARTESIAN_POINT ( 'NONE',  ( -1.737328882695368115, 14.25515036105620581, 26.63881657323070939 ) ) ;
#4766 = CARTESIAN_POINT ( 'NONE',  ( -7.842167650704559456, -7.771249796623176387, 7.251137918078588207 ) ) ;
#4767 = CARTESIAN_POINT ( 'NONE',  ( -4.355403765523468529, -8.442910196168346815, 10.10113791807856742 ) ) ;
#4768 = DIRECTION ( 'NONE',  ( -1.000000000000000000, 1.842239752758738928E-31, -1.780435181894459419E-32 ) ) ;
#4769 = CARTESIAN_POINT ( 'NONE',  ( -13.92619789766827054, -1.441234910513399470, 3.146897712483577969 ) ) ;
#4770 = CARTESIAN_POINT ( 'NONE',  ( 7.529642458189280241, -12.22833218042435099, 7.218326283912148256 ) ) ;
#4771 = VERTEX_POINT ( 'NONE', #253 ) ;
#4772 = CARTESIAN_POINT ( 'NONE',  ( -70.00000000000001421, 0.000000000000000000, 0.000000000000000000 ) ) ;
#4773 = CARTESIAN_POINT ( 'NONE',  ( 11.31370849898469899, 11.31370849898481978, 49.50000000000000711 ) ) ;
#4774 = DIRECTION ( 'NONE',  ( 0.7071067811865431318, 0.7071067811865519026, -7.359808400080253795E-17 ) ) ;
#4775 = LINE ( 'NONE', #5393, #4131 ) ;
#4776 = CARTESIAN_POINT ( 'NONE',  ( -4.534861676072319270, 8.900167166472117586, 18.15000000000000924 ) ) ;
#4777 = CARTESIAN_POINT ( 'NONE',  ( -1.486127417882243895, 9.383039235653825472, 9.299999999999975842 ) ) ;
#4778 = CARTESIAN_POINT ( 'NONE',  ( -166.8656692072818828, 1.077730084761960194, 12.95578054544406044 ) ) ;
#4779 = CARTESIAN_POINT ( 'NONE',  ( 8.464561979789474222, 4.312909747525755400, 3.899999999999959055 ) ) ;
#4780 = CARTESIAN_POINT ( 'NONE',  ( 11.69682198916835070, 11.51250119794901394, 29.50404056962643295 ) ) ;
#4781 = ORIENTED_EDGE ( 'NONE', *, *, #4544, .T. ) ;
#4782 = AXIS2_PLACEMENT_3D ( 'NONE', #2144, #5349, #5291 ) ;
#4783 = CARTESIAN_POINT ( 'NONE',  ( 1.791431617652837316, 15.89939535829188877, 30.85714285714286120 ) ) ;
#4784 = DIRECTION ( 'NONE',  ( 0.000000000000000000, 0.000000000000000000, 1.000000000000000000 ) ) ;
#4785 = CARTESIAN_POINT ( 'NONE',  ( 13.54758718765249803, 8.512513224245457977, 7.714285714285715301 ) ) ;
#4786 = CARTESIAN_POINT ( 'NONE',  ( -1.513077731352923339, -9.873755945037078874, 2.948862081921438616 ) ) ;
#4787 = CARTESIAN_POINT ( 'NONE',  ( -7.771249796623103556, -7.842167650704634063, 15.24886208192144110 ) ) ;
#4788 = CARTESIAN_POINT ( 'NONE',  ( -5.543385399275643444, -15.44746603149420494, 2.075469141055009015 ) ) ;
#4789 = AXIS2_PLACEMENT_3D ( 'NONE', #3397, #5617, #8837 ) ;
#4790 = CARTESIAN_POINT ( 'NONE',  ( -5.284464991282755264, 15.10213328493384743, 12.42857142857142705 ) ) ;
#4791 = CONTEXT_DEPENDENT_SHAPE_REPRESENTATION ( #3086, #8286 ) ;
#4792 = AXIS2_PLACEMENT_3D ( 'NONE', #7204, #9595, #2601 ) ;
#4793 = CARTESIAN_POINT ( 'NONE',  ( -4.623906867372410190, 13.21436662431711895, 42.42857142857143060 ) ) ;
#4794 = CARTESIAN_POINT ( 'NONE',  ( 7.529642458189280241, -12.22833218042435099, 37.21832628391215536 ) ) ;
#4795 = CARTESIAN_POINT ( 'NONE',  ( -7.556039541191334585, -11.78653521626503320, 32.28975485534072476 ) ) ;
#4796 = CARTESIAN_POINT ( 'NONE',  ( 9.865911304835478290, 1.562606840307950273, 10.05000000000003268 ) ) ;
#4797 = CARTESIAN_POINT ( 'NONE',  ( -10.37072757624895836, 1.642561882922380034, 14.69999999999999041 ) ) ;
#4798 = ORIENTED_EDGE ( 'NONE', *, *, #5975, .T. ) ;
#4799 = CARTESIAN_POINT ( 'NONE',  ( 1.607813917173038121, -14.26974319298267346, 3.642857142857144126 ) ) ;
#4800 = AXIS2_PLACEMENT_3D ( 'NONE', #8667, #1589, #7108 ) ;
#4801 = VECTOR ( 'NONE', #3746, 1000.000000000000114 ) ;
#4802 = FACE_OUTER_BOUND ( 'NONE', #9503, .T. ) ;
#4803 = AXIS2_PLACEMENT_3D ( 'NONE', #7447, #372, #9834 ) ;
#4804 = CARTESIAN_POINT ( 'NONE',  ( 15.49051278174637858, 5.420364854932174126, 19.92857142857143415 ) ) ;
#4805 = CARTESIAN_POINT ( 'NONE',  ( -8.404922754268618235, -13.61519076058357491, 42.28167371608785174 ) ) ;
#4806 = CARTESIAN_POINT ( 'NONE',  ( 61.99999999999997158, 9.797174393178825657E-16, -8.000000000000000000 ) ) ;
#4807 = CARTESIAN_POINT ( 'NONE',  ( 7.424621202458790314, -7.424621202458697944, 4.500000000000003553 ) ) ;
#4808 = LINE ( 'NONE', #51, #6275 ) ;
#4809 = CIRCLE ( 'NONE', #7088, 15.44569104238500046 ) ;
#4810 = SURFACE_STYLE_FILL_AREA ( #153 ) ;
#4811 = ORIENTED_EDGE ( 'NONE', *, *, #987, .F. ) ;
#4812 = CARTESIAN_POINT ( 'NONE',  ( -14.28433602490915000, 1.478298951650542481, 19.35310228751642825 ) ) ;
#4813 = CARTESIAN_POINT ( 'NONE',  ( 1.727091770866551412, 10.90442828429187117, 9.449999999999992184 ) ) ;
#4814 = ADVANCED_FACE ( 'NONE', ( #9900 ), #10001, .F. ) ;
#4815 = CARTESIAN_POINT ( 'NONE',  ( -163.9856078553142709, 1.318997900831586856, 12.93381406529030642 ) ) ;
#4816 = CARTESIAN_POINT ( 'NONE',  ( 11.78653521626494793, 7.556039541191463371, 27.71024514465928235 ) ) ;
#4817 = CARTESIAN_POINT ( 'NONE',  ( -1.776620879821455556, -10.89658364409025992, 3.951137918078560851 ) ) ;
#4818 = CARTESIAN_POINT ( 'NONE',  ( -1.612135949262737844, -9.858066664633888365, 15.95113791807857595 ) ) ;
#4819 = CARTESIAN_POINT ( 'NONE',  ( -4.169902070941136074, -13.58603705635637482, 0.000000000000000000 ) ) ;
#4820 = CARTESIAN_POINT ( 'NONE',  ( -7.529642458189277576, 12.22833218042435455, 4.218326283912150032 ) ) ;
#4821 = CARTESIAN_POINT ( 'NONE',  ( -14.25515036105622890, 1.737328882695209575, 15.36118342676929771 ) ) ;
#4822 = ORIENTED_EDGE ( 'NONE', *, *, #3450, .F. ) ;
#4823 = CARTESIAN_POINT ( 'NONE',  ( 16.00000000000000000, 1.959434878635765131E-15, 68.00000000000000000 ) ) ;
#4824 = CARTESIAN_POINT ( 'NONE',  ( -15.10213328493390961, 5.284464991282586510, 41.57142857142856940 ) ) ;
#4825 = CARTESIAN_POINT ( 'NONE',  ( -164.7848126586117985, -1.639441178260655052, 12.89622722885275152 ) ) ;
#4826 = DIRECTION ( 'NONE',  ( 0.000000000000000000, 8.191099868251446680E-34, 1.000000000000000000 ) ) ;
#4827 = CARTESIAN_POINT ( 'NONE',  ( 1.486127417882244783, -9.383039235653791721, 13.80000000000003446 ) ) ;
#4828 = CARTESIAN_POINT ( 'NONE',  ( 8.464561979789474222, 4.312909747525755400, 9.900000000000019895 ) ) ;
#4829 = CARTESIAN_POINT ( 'NONE',  ( -163.3796219069818960, 1.420182798501361754, 12.92258649737903298 ) ) ;
#4830 = CARTESIAN_POINT ( 'NONE',  ( 5.164528828830335705, -15.14410076328347543, 25.43261199819786711 ) ) ;
#4831 = CARTESIAN_POINT ( 'NONE',  ( 1.486127417882244783, -9.383039235653791721, 4.800000000000026468 ) ) ;
#4832 = CARTESIAN_POINT ( 'NONE',  ( 16.29368510291089223, -1.967016585148476882, 30.36118342676929771 ) ) ;
#4833 = ORIENTED_EDGE ( 'NONE', *, *, #5587, .T. ) ;
#4834 = CARTESIAN_POINT ( 'NONE',  ( -13.89598863503046111, 8.731428362939027465, 35.78571428571429180 ) ) ;
#4835 = CARTESIAN_POINT ( 'NONE',  ( 3.908916549244207506, 14.54798010869238567, 2.434022981070398982E-13 ) ) ;
#4836 = AXIS2_PLACEMENT_3D ( 'NONE', #4879, #7401, #5029 ) ;
#4837 = CARTESIAN_POINT ( 'NONE',  ( 8.512513224245308763, 13.54758718765259040, 1.285714285714285809 ) ) ;
#4838 = EDGE_CURVE ( 'NONE', #1178, #6635, #3521, .T. ) ;
#4839 = CARTESIAN_POINT ( 'NONE',  ( -170.0000000000000284, -8.084771497730068080E-15, 0.000000000000000000 ) ) ;
#4840 = CARTESIAN_POINT ( 'NONE',  ( -6.751237864895158758, 6.683790977649261222, 6.998862081921422451 ) ) ;
#4841 = CARTESIAN_POINT ( 'NONE',  ( -10.37818827243067688, 1.595456901104524761, 15.69886208192145816 ) ) ;
#4842 = AXIS2_PLACEMENT_3D ( 'NONE', #21, #6993, #8501 ) ;
#4843 = CARTESIAN_POINT ( 'NONE',  ( 11.22385875690717683, -11.40355824106234373, 1.004040569626440726 ) ) ;
#4844 = CARTESIAN_POINT ( 'NONE',  ( 11.31370849898482334, -11.31370849898469366, 21.00000000000000355 ) ) ;
#4845 = CARTESIAN_POINT ( 'NONE',  ( 9.899494936611718643, -9.899494936611608509, 33.00000000000000000 ) ) ;
#4846 = CARTESIAN_POINT ( 'NONE',  ( 12.08964793087886314, -7.750357176954162597, 36.78975485534072476 ) ) ;
#4847 = CARTESIAN_POINT ( 'NONE',  ( 1.567502665446232957, 13.91197093850540156, 6.857142857142860315 ) ) ;
#4848 = CARTESIAN_POINT ( 'NONE',  ( -1.486127417882243895, 9.383039235653816590, 18.29999999999998295 ) ) ;
#4849 = CARTESIAN_POINT ( 'NONE',  ( 9.333916720356675967, 4.809394265263123636, 10.89886208192140771 ) ) ;
#4850 = VERTEX_POINT ( 'NONE', #4469 ) ;
#4851 = CARTESIAN_POINT ( 'NONE',  ( 7.448449071214646722, 11.85413878919601594, 7.285714285714284699 ) ) ;
#4852 = VERTEX_POINT ( 'NONE', #598 ) ;
#4853 = CARTESIAN_POINT ( 'NONE',  ( -58.00000000000002842, 7.703719777548943412E-30, -1.059261469412979719E-30 ) ) ;
#4854 = VECTOR ( 'NONE', #3214, 1000.000000000000114 ) ;
#4855 = CARTESIAN_POINT ( 'NONE',  ( -1.837501619626327853, 16.30827793483733856, 12.64285714285714235 ) ) ;
#4856 = PRODUCT_RELATED_PRODUCT_CATEGORY ( 'part', '', ( #5087 ) ) ;
#4857 = CARTESIAN_POINT ( 'NONE',  ( 15.14410076328353227, -5.164528828830166063, 34.56738800180213644 ) ) ;
#4858 = CARTESIAN_POINT ( 'NONE',  ( 9.355568503977840678, 4.766900247265305701, 3.899999999999959055 ) ) ;
#4859 = CARTESIAN_POINT ( 'NONE',  ( 9.837026868206066865, -5.012215536711392083, 7.350000000000000533 ) ) ;
#4860 = CARTESIAN_POINT ( 'NONE',  ( 13.55419868402807992, 4.742819248065649695, 1.928571428571430380 ) ) ;
#4861 = EDGE_CURVE ( 'NONE', #7065, #3486, #7624, .T. ) ;
#4862 = VERTEX_POINT ( 'NONE', #544 ) ;
#4863 = CARTESIAN_POINT ( 'NONE',  ( -7.340858601237953529, -11.92174236212700222, 12.28167371608784997 ) ) ;
#4864 = CARTESIAN_POINT ( 'NONE',  ( -10.90442828429184274, -1.727091770866655107, 17.55000000000002913 ) ) ;
#4865 = CARTESIAN_POINT ( 'NONE',  ( 1.837501619626330074, -16.30827793483733501, 9.642857142857147679 ) ) ;
#4866 = CARTESIAN_POINT ( 'NONE',  ( -163.7574652328086131, 1.090948703523729746, 12.95436823472124566 ) ) ;
#4867 = CARTESIAN_POINT ( 'NONE',  ( 5.420364854932001819, 15.49051278174644430, 37.07142857142857650 ) ) ;
#4868 = CARTESIAN_POINT ( 'NONE',  ( 7.340858601237956194, 11.92174236212700045, 33.28167371608784464 ) ) ;
#4869 = CARTESIAN_POINT ( 'NONE',  ( -10.36326688006724162, 1.689666864740236862, 10.70113791807854220 ) ) ;
#4870 = CARTESIAN_POINT ( 'NONE',  ( 1.612135949262739398, 9.858066664633913234, 17.45113791807857240 ) ) ;
#4871 = CARTESIAN_POINT ( 'NONE',  ( 2.000000000000001776, 0.8865213383407039016, -1.535500000000022958 ) ) ;
#4872 = CARTESIAN_POINT ( 'NONE',  ( 12.08964793087886314, -7.750357176954162597, 6.789754855340717654 ) ) ;
#4873 = APPLICATION_CONTEXT ( 'automotive_design' ) ;
#4874 = CARTESIAN_POINT ( 'NONE',  ( 4.503970704919991519, -13.25633410266674517, 7.432611998197861780 ) ) ;
#4875 = ORIENTED_EDGE ( 'NONE', *, *, #6005, .T. ) ;
#4876 = EDGE_CURVE ( 'NONE', #557, #1035, #7975, .T. ) ;
#4877 = CARTESIAN_POINT ( 'NONE',  ( -160.0000000000000284, -7.609196703745946707E-15, 0.000000000000000000 ) ) ;
#4878 = CARTESIAN_POINT ( 'NONE',  ( 1.967016585148662289, -16.29368510291087091, 11.63881657323070939 ) ) ;
#4879 = CARTESIAN_POINT ( 'NONE',  ( -58.00000000000002842, 7.703719777548943412E-30, -1.059261469412979719E-30 ) ) ;
#4880 = DIRECTION ( 'NONE',  ( -4.755747939841215952E-17, 1.000000000000000000, 0.000000000000000000 ) ) ;
#4881 = CARTESIAN_POINT ( 'NONE',  ( -6.683790977649319842, 6.751237864895101026, -0.9988620819214586444 ) ) ;
#4882 = CARTESIAN_POINT ( 'NONE',  ( -8.464561979789474222, -4.312909747525728754, 5.400000000000016342 ) ) ;
#4883 = CARTESIAN_POINT ( 'NONE',  ( 4.200000000000009059, 0.000000000000000000, 0.000000000000000000 ) ) ;
#4884 = CARTESIAN_POINT ( 'NONE',  ( 11.22385875690717683, -11.40355824106234373, 25.00404056962644006 ) ) ;
#4885 = CARTESIAN_POINT ( 'NONE',  ( 8.464561979789474222, 4.312909747525755400, 0.9000000000000119016 ) ) ;
#4886 = CARTESIAN_POINT ( 'NONE',  ( -15.06016580658428694, 5.404401153735006957, 33.57546914105500946 ) ) ;
#4887 = EDGE_LOOP ( 'NONE', ( #8548, #9088, #1137, #10177 ) ) ;
#4888 = CARTESIAN_POINT ( 'NONE',  ( 13.89598863503046111, -8.731428362939032795, 32.78571428571430602 ) ) ;
#4889 = CARTESIAN_POINT ( 'NONE',  ( 3.436234746893573444, 14.87838136757911656, 2.020632658447805774E-13 ) ) ;
#4890 = CARTESIAN_POINT ( 'NONE',  ( 5.420364854932001819, 15.49051278174644430, 7.071428571428569398 ) ) ;
#4891 = DIRECTION ( 'NONE',  ( 0.000000000000000000, 0.000000000000000000, 1.000000000000000000 ) ) ;
#4892 = CARTESIAN_POINT ( 'NONE',  ( -6.751237864895158758, 6.683790977649260334, 9.998862081921425116 ) ) ;
#4893 = CARTESIAN_POINT ( 'NONE',  ( -9.333916720356675967, -4.809394265263096990, 18.39886208192140771 ) ) ;
#4894 = CARTESIAN_POINT ( 'NONE',  ( 8.620103694221997515, 13.47998361472160767, -0.7102451446592792372 ) ) ;
#4895 = CARTESIAN_POINT ( 'NONE',  ( -11.31370849898482156, 11.31370849898469544, 11.99999999999999645 ) ) ;
#4896 = CARTESIAN_POINT ( 'NONE',  ( -14.26974319298268767, 1.607813917172874696, 41.35714285714286120 ) ) ;
#4897 = CARTESIAN_POINT ( 'NONE',  ( -9.809645194534070356, 9.989344678689256796, 40.00404056962644006 ) ) ;
#4898 = CARTESIAN_POINT ( 'NONE',  ( 13.55419868402807992, 4.742819248065648807, 13.92857142857143238 ) ) ;
#4899 = DIRECTION ( 'NONE',  ( 0.2882273949230689802, 0.9575619921529161527, -1.755378125195851735E-33 ) ) ;
#4900 = CARTESIAN_POINT ( 'NONE',  ( 10.89658364409024749, 1.776620879821585897, 8.048862081921450695 ) ) ;
#4901 = VERTEX_POINT ( 'NONE', #2300 ) ;
#4902 = CARTESIAN_POINT ( 'NONE',  ( -7.448449071214644945, -11.85413878919601771, 4.285714285714288252 ) ) ;
#4903 = CARTESIAN_POINT ( 'NONE',  ( -43.00000000000002842, 8.200000000000018829, 8.906797881070005341E-17 ) ) ;
#4904 = VECTOR ( 'NONE', #9324, 1000.000000000000000 ) ;
#4905 = EDGE_CURVE ( 'NONE', #4150, #4862, #10106, .T. ) ;
#4906 = CARTESIAN_POINT ( 'NONE',  ( -5.420364854931998266, -15.49051278174643898, 22.07142857142858006 ) ) ;
#4907 = CARTESIAN_POINT ( 'NONE',  ( 15.14410076328353227, -5.164528828830166063, 40.56738800180214355 ) ) ;
#4908 = CARTESIAN_POINT ( 'NONE',  ( -1.727091770866549414, -10.90442828429184274, 7.950000000000040146 ) ) ;
#4909 = CARTESIAN_POINT ( 'NONE',  ( 10.90442828429183919, 1.727091770866678422, 4.049999999999988276 ) ) ;
#4910 = CARTESIAN_POINT ( 'NONE',  ( 7.639999817571788476, -12.15899005565156266, 3.214285714285716633 ) ) ;
#4911 = AXIS2_PLACEMENT_3D ( 'NONE', #3043, #8576, #7806 ) ;
#4912 = ORIENTED_EDGE ( 'NONE', *, *, #2903, .T. ) ;
#4913 = CARTESIAN_POINT ( 'NONE',  ( 11.78653521626494793, 7.556039541191463371, 9.710245144659278793 ) ) ;
#4914 = CARTESIAN_POINT ( 'NONE',  ( 4.766900247265192903, 9.355568503977911732, 9.599999999999997868 ) ) ;
#4915 = CARTESIAN_POINT ( 'NONE',  ( -13.54758718765249625, -8.512513224245459753, 10.71428571428571708 ) ) ;
#4916 = CARTESIAN_POINT ( 'NONE',  ( 11.48991645990273724, -11.34085470199652512, 0.000000000000000000 ) ) ;
#4917 = EDGE_CURVE ( 'NONE', #7065, #6270, #6149, .T. ) ;
#4918 = CARTESIAN_POINT ( 'NONE',  ( -5.284464991282755264, 15.10213328493384743, 36.42857142857143060 ) ) ;
#4919 = CARTESIAN_POINT ( 'NONE',  ( 7.750357176954296712, -12.08964793087877787, 35.21024514465927524 ) ) ;
#4920 = CARTESIAN_POINT ( 'NONE',  ( 4.809394265263009061, 9.333916720356739916, 17.60113791807856742 ) ) ;
#4921 = CARTESIAN_POINT ( 'NONE',  ( 4.355403765523470305, 8.442910196168369907, 17.60113791807856742 ) ) ;
#4922 = DIRECTION ( 'NONE',  ( -1.000000000000000000, 1.842239752758738928E-31, -1.780435181894459419E-32 ) ) ;
#4923 = CARTESIAN_POINT ( 'NONE',  ( 10.24623928997352884, 10.06191849875416899, 23.50404056962643295 ) ) ;
#4924 = CARTESIAN_POINT ( 'NONE',  ( 4.865839792409144771, 13.51115193377589740, 11.07546914105500768 ) ) ;
#4925 = CARTESIAN_POINT ( 'NONE',  ( -0.9669241168434388189, 13.98238843080921079, 48.73000000000005372 ) ) ;
#4926 = CARTESIAN_POINT ( 'NONE',  ( 15.14410076328353227, -5.164528828830166063, 10.56738800180213644 ) ) ;
#4927 = PRODUCT_DEFINITION_FORMATION_WITH_SPECIFIED_SOURCE ( 'ANY', '', #9883, .NOT_KNOWN. ) ;
#4928 = CARTESIAN_POINT ( 'NONE',  ( -164.4688726891355088, -1.565914946704515254, 12.90541139627661593 ) ) ;
#4929 = CARTESIAN_POINT ( 'NONE',  ( -163.6882045205299789, -1.709201878644992956, 14.90250977739813365 ) ) ;
#4930 = CARTESIAN_POINT ( 'NONE',  ( -1.612135949262737844, -9.858066664633893694, 3.951137918078560851 ) ) ;
#4931 = CARTESIAN_POINT ( 'NONE',  ( 4.534861676072320158, -8.900167166472098046, 1.650000000000006128 ) ) ;
#4932 = DIRECTION ( 'NONE',  ( 1.000000000000000000, 0.000000000000000000, 0.000000000000000000 ) ) ;
#4933 = CARTESIAN_POINT ( 'NONE',  ( 13.61519076058348254, 8.404922754268771001, 29.71832628391214826 ) ) ;
#4934 = CARTESIAN_POINT ( 'NONE',  ( -4.742819248065502258, -13.55419868402813677, 34.07142857142859071 ) ) ;
#4935 = CARTESIAN_POINT ( 'NONE',  ( 15.06016580658428694, -5.404401153735007846, 36.57546914105501656 ) ) ;
#4936 = ORIENTED_EDGE ( 'NONE', *, *, #6195, .F. ) ;
#4937 = CARTESIAN_POINT ( 'NONE',  ( -1.791431617652833763, -15.89939535829188877, 33.85714285714285410 ) ) ;
#4938 = CARTESIAN_POINT ( 'NONE',  ( -9.899494936611716867, 9.899494936611610285, 0.000000000000000000 ) ) ;
#4939 = CARTESIAN_POINT ( 'NONE',  ( -11.60466159355861926, -11.60466159355875249, 22.50000000000000000 ) ) ;
#4940 = SURFACE_STYLE_FILL_AREA ( #9657 ) ;
#4941 = CARTESIAN_POINT ( 'NONE',  ( 9.383039235653818366, -1.486127417882130208, 1.200000000000034373 ) ) ;
#4942 = CARTESIAN_POINT ( 'NONE',  ( 9.859792900771104485, -4.967534682030585458, 14.34886208192142831 ) ) ;
#4943 = UNCERTAINTY_MEASURE_WITH_UNIT (LENGTH_MEASURE( 1.000000000000000082E-05 ), #9420, 'distance_accuracy_value', 'NONE');
#4944 = CARTESIAN_POINT ( 'NONE',  ( 1.478298951650704351, -14.28433602490913579, 43.64689771248358596 ) ) ;
#4945 = CARTESIAN_POINT ( 'NONE',  ( 11.31370849898482334, -11.31370849898469366, 33.00000000000000000 ) ) ;
#4946 = CARTESIAN_POINT ( 'NONE',  ( 0.000000000000000000, 0.000000000000000000, 0.000000000000000000 ) ) ;
#4947 = CARTESIAN_POINT ( 'NONE',  ( 9.809645194534072132, -9.989344678689256796, 43.00404056962644717 ) ) ;
#4948 = EDGE_CURVE ( 'NONE', #166, #2905, #52, .T. ) ;
#4949 = CARTESIAN_POINT ( 'NONE',  ( 15.89939535829187278, 1.791431617653015174, 38.14285714285714590 ) ) ;
#4950 = CARTESIAN_POINT ( 'NONE',  ( 14.00000000000000533, 0.000000000000000000, 0.000000000000000000 ) ) ;
#4951 = CARTESIAN_POINT ( 'NONE',  ( -7.458344646081709328, 7.390897758835799358, 3.998862081921419342 ) ) ;
#4952 = ORIENTED_EDGE ( 'NONE', *, *, #1997, .F. ) ;
#4953 = CARTESIAN_POINT ( 'NONE',  ( 9.899494936611718643, -9.899494936611608509, 21.00000000000000355 ) ) ;
#4954 = VERTEX_POINT ( 'NONE', #9442 ) ;
#4955 = DIRECTION ( 'NONE',  ( -4.755747939841215952E-17, 1.000000000000000000, 0.000000000000000000 ) ) ;
#4956 = CARTESIAN_POINT ( 'NONE',  ( 8.731428362939189114, -13.89598863503035986, 21.21428571428571530 ) ) ;
#4957 = CIRCLE ( 'NONE', #6430, 18.00000000000002132 ) ;
#4958 = CARTESIAN_POINT ( 'NONE',  ( 5.404401153735178376, -15.06016580658422477, 41.42453085894499765 ) ) ;
#4959 = CARTESIAN_POINT ( 'NONE',  ( 5.012215536711511987, -9.837026868205999364, 4.650000000000026112 ) ) ;
#4960 = CARTESIAN_POINT ( 'NONE',  ( 1.642561882922480621, -10.37072757624892638, 13.80000000000003446 ) ) ;
#4961 = CARTESIAN_POINT ( 'NONE',  ( -9.899494936611716867, 9.899494936611610285, 18.00000000000000355 ) ) ;
#4962 = VECTOR ( 'NONE', #3339, 1000.000000000000000 ) ;
#4963 = STYLED_ITEM ( 'NONE', ( #9754 ), #7117 ) ;
#4964 = CIRCLE ( 'NONE', #3310, 16.00000000000000000 ) ;
#4965 = CARTESIAN_POINT ( 'NONE',  ( 13.51115193377584589, 4.865839792409294873, 15.92453085894499409 ) ) ;
#4966 = ORIENTED_EDGE ( 'NONE', *, *, #9912, .T. ) ;
#4967 = CARTESIAN_POINT ( 'NONE',  ( 1.642561882922480621, -10.37072757624891750, 10.80000000000003268 ) ) ;
#4968 = CARTESIAN_POINT ( 'NONE',  ( -58.00000000000001421, 1.004210375300829674E-15, -8.200000000000001066 ) ) ;
#4969 = ADVANCED_FACE ( 'NONE', ( #4727 ), #2349, .T. ) ;
#4970 = CARTESIAN_POINT ( 'NONE',  ( 13.25633410266679313, -4.503970704919842305, 40.56738800180214355 ) ) ;
#4971 = CARTESIAN_POINT ( 'NONE',  ( 1.776620879821457333, 10.89658364409028124, 17.45113791807857240 ) ) ;
#4972 = CARTESIAN_POINT ( 'NONE',  ( 9.377220287599001836, 4.724406229267489543, 8.901137918078571687 ) ) ;
#4973 = AXIS2_PLACEMENT_3D ( 'NONE', #4839, #1789, #3188 ) ;
#4974 = CARTESIAN_POINT ( 'NONE',  ( 0.000000000000000000, 0.000000000000000000, 0.000000000000000000 ) ) ;
#4975 = CARTESIAN_POINT ( 'NONE',  ( 11.92174236212692229, 7.340858601238088532, 17.71832628391214826 ) ) ;
#4976 = CARTESIAN_POINT ( 'NONE',  ( -7.529642458189277576, 12.22833218042435455, 22.21832628391215181 ) ) ;
#4977 = CARTESIAN_POINT ( 'NONE',  ( 2.000000000000001776, 1.773042676681366281, 0.000000000000000000 ) ) ;
#4978 = CARTESIAN_POINT ( 'NONE',  ( 8.841785722321695573, -13.82664651025757152, 5.210245144659280569 ) ) ;
#4979 = CARTESIAN_POINT ( 'NONE',  ( -166.4422304502845407, -0.8298597800914565559, 12.97500904825187540 ) ) ;
#4980 = CARTESIAN_POINT ( 'NONE',  ( -166.0759530565494231, -1.866699619213640027, 14.88360162420890020 ) ) ;
#4981 = ADVANCED_FACE ( 'NONE', ( #5348 ), #5499, .T. ) ;
#4982 = CARTESIAN_POINT ( 'NONE',  ( -1.612135949262737844, -9.858066664633888365, 9.951137918078590161 ) ) ;
#4983 = CARTESIAN_POINT ( 'NONE',  ( -7.063212654743466601, -7.063212654743531438, 14.25000000000001243 ) ) ;
#4984 = DIRECTION ( 'NONE',  ( 0.000000000000000000, -6.338944243255235518E-49, 1.000000000000000000 ) ) ;
#4985 = CARTESIAN_POINT ( 'NONE',  ( -11.22385875690717327, 11.40355824106234550, 40.00404056962644006 ) ) ;
#4986 = CLOSED_SHELL ( 'NONE', ( #3836, #9463, #394, #3143, #7435, #8404, #992, #609, #6555, #3646, #9871, #6343, #4981, #1510, #2264, #4814 ) ) ;
#4987 = CARTESIAN_POINT ( 'NONE',  ( -7.448449071214644945, -11.85413878919601771, 28.28571428571428825 ) ) ;
#4988 = CARTESIAN_POINT ( 'NONE',  ( 15.91362231745475597, 1.665163862720026255, 42.14689771248358596 ) ) ;
#4989 = VERTEX_POINT ( 'NONE', #9387 ) ;
#4990 = CARTESIAN_POINT ( 'NONE',  ( -11.60466159355861926, -11.60466159355875249, 34.50000000000000000 ) ) ;
#4991 = CARTESIAN_POINT ( 'NONE',  ( 2.601377816629832473, 14.36985073060440499, 7.004981435163793185E-16 ) ) ;
#4992 = CARTESIAN_POINT ( 'NONE',  ( 11.31370849898482334, -11.31370849898469366, 21.00000000000000355 ) ) ;
#4993 = CARTESIAN_POINT ( 'NONE',  ( 4.000000000000003553, 0.000000000000000000, 0.000000000000000000 ) ) ;
#4994 = CARTESIAN_POINT ( 'NONE',  ( -4.534861676072319270, 8.900167166472121139, 0.1499999999999952482 ) ) ;
#4995 = CARTESIAN_POINT ( 'NONE',  ( 10.89658364409024749, 1.776620879821585897, 17.04886208192142760 ) ) ;
#4996 = CARTESIAN_POINT ( 'NONE',  ( -15.91362231745475597, -1.665163862720028254, 15.14689771248357708 ) ) ;
#4997 = CARTESIAN_POINT ( 'NONE',  ( 15.10213328493390783, -5.284464991282587398, 32.57142857142856940 ) ) ;
#4998 = CARTESIAN_POINT ( 'NONE',  ( 13.61519076058348254, 8.404922754268771001, 5.718326283912152697 ) ) ;
#4999 = AXIS2_PLACEMENT_3D ( 'NONE', #2498, #2643, #8126 ) ;
#5000 = CARTESIAN_POINT ( 'NONE',  ( 11.85413878919593422, 7.448449071214774619, 7.714285714285715301 ) ) ;
#5001 = CARTESIAN_POINT ( 'NONE',  ( -4.534861676072319270, 8.900167166472122915, 15.14999999999998614 ) ) ;
#5002 = CARTESIAN_POINT ( 'NONE',  ( 7.771249796623105333, 7.842167650704653603, 4.748862081921425116 ) ) ;
#5003 = ORIENTED_EDGE ( 'NONE', *, *, #9284, .F. ) ;
#5004 = CARTESIAN_POINT ( 'NONE',  ( -13.21436662431716869, 4.623906867372262752, 17.57142857142856940 ) ) ;
#5005 = ORIENTED_EDGE ( 'NONE', *, *, #13, .T. ) ;
#5006 = CARTESIAN_POINT ( 'NONE',  ( 1.837501619626329630, -16.30827793483733501, 27.64285714285714590 ) ) ;
#5007 = CARTESIAN_POINT ( 'NONE',  ( 16.32287076676382043, -1.707986654103810897, 34.35310228751642825 ) ) ;
#5008 =( REPRESENTATION_RELATIONSHIP ('NONE','NONE', #58, #1047 ) REPRESENTATION_RELATIONSHIP_WITH_TRANSFORMATION ( #1493 )SHAPE_REPRESENTATION_RELATIONSHIP( ) );
#5009 = CARTESIAN_POINT ( 'NONE',  ( 1.727091770866550968, 10.90442828429186761, 6.449999999999969091 ) ) ;
#5010 = CARTESIAN_POINT ( 'NONE',  ( 7.448449071214646722, 11.85413878919601594, 7.285714285714284699 ) ) ;
#5011 = CARTESIAN_POINT ( 'NONE',  ( -4.743843029824828861, 13.17239914596749450, 26.42453085894499765 ) ) ;
#5012 = ORIENTED_EDGE ( 'NONE', *, *, #7460, .F. ) ;
#5013 = CARTESIAN_POINT ( 'NONE',  ( -88.00000000000002842, 9.797174393178825657E-16, -8.000000000000000000 ) ) ;
#5014 = CARTESIAN_POINT ( 'NONE',  ( -165.1071317273496959, 1.650039592648423259, 12.89485825219862569 ) ) ;
#5015 = CARTESIAN_POINT ( 'NONE',  ( -10.06191849875405531, -10.24623928997363542, 42.49595943037355994 ) ) ;
#5016 = CARTESIAN_POINT ( 'NONE',  ( -4.967534682030703586, 9.859792900771058299, 14.15113791807854327 ) ) ;
#5017 = CARTESIAN_POINT ( 'NONE',  ( -10.36326688006724162, 1.689666864740236640, 4.701137918078535982 ) ) ;
#5018 = VECTOR ( 'NONE', #7541, 1000.000000000000000 ) ;
#5019 = CARTESIAN_POINT ( 'NONE',  ( 0.2000000000000057288, 2.866884953888006423E-33, 3.500000000000000000 ) ) ;
#5020 = CARTESIAN_POINT ( 'NONE',  ( -11.92174236212692051, -7.340858601238089420, 20.71832628391214826 ) ) ;
#5021 = ADVANCED_FACE ( 'NONE', ( #3175 ), #651, .F. ) ;
#5022 = CARTESIAN_POINT ( 'NONE',  ( -7.556039541191334585, -11.78653521626503320, 26.28975485534072831 ) ) ;
#5023 = CARTESIAN_POINT ( 'NONE',  ( 10.37072757624895836, -1.642561882922355609, 7.199999999999984190 ) ) ;
#5024 = CARTESIAN_POINT ( 'NONE',  ( -1.665163862719845067, -15.91362231745477374, 41.85310228751642825 ) ) ;
#5025 = ORIENTED_EDGE ( 'NONE', *, *, #5600, .F. ) ;
#5026 = CARTESIAN_POINT ( 'NONE',  ( -2.927791565357304115, 15.72098899558116436, 48.73000000000027399 ) ) ;
#5027 = CARTESIAN_POINT ( 'NONE',  ( -1.837501619626328297, 16.30827793483733856, 18.64285714285715656 ) ) ;
#5028 = CARTESIAN_POINT ( 'NONE',  ( -15.44746603149413922, -5.543385399275820191, 12.92453085894499587 ) ) ;
#5029 = DIRECTION ( 'NONE',  ( 0.000000000000000000, 6.938893903907221444E-18, 1.000000000000000000 ) ) ;
#5030 = CARTESIAN_POINT ( 'NONE',  ( -166.3097507274169686, -1.710787970585769813, 14.90232764692231271 ) ) ;
#5031 = CARTESIAN_POINT ( 'NONE',  ( -1.439022436064386845, 9.390499931835535108, 5.301137918078554279 ) ) ;
#5032 = CARTESIAN_POINT ( 'NONE',  ( 6.717514421272239744, -6.717514421272154479, 19.50000000000001776 ) ) ;
#5033 = FACE_OUTER_BOUND ( 'NONE', #3921, .T. ) ;
#5034 = CARTESIAN_POINT ( 'NONE',  ( -16.29368510291090288, 1.967016585148476215, 33.36118342676929416 ) ) ;
#5035 = CARTESIAN_POINT ( 'NONE',  ( -1.567502665446231180, -13.91197093850540334, 33.85714285714285410 ) ) ;
#5036 = CARTESIAN_POINT ( 'NONE',  ( 13.91197093850538380, 1.567502665446386390, 38.14285714285714590 ) ) ;
#5037 = ORIENTED_EDGE ( 'NONE', *, *, #9692, .T. ) ;
#5038 = CARTESIAN_POINT ( 'NONE',  ( -5.284464991282755264, 15.10213328493384743, 48.42857142857143060 ) ) ;
#5039 = CARTESIAN_POINT ( 'NONE',  ( 6.919986107680329290, -12.02850919814119379, -1.270000000000007123 ) ) ;
#5040 = CARTESIAN_POINT ( 'NONE',  ( 5.284464991282756152, -15.10213328493384743, 21.42857142857142705 ) ) ;
#5041 = CYLINDRICAL_SURFACE ( 'NONE', #1832, 8.500000000000000000 ) ;
#5042 = PLANE ( 'NONE',  #3474 ) ;
#5043 = CARTESIAN_POINT ( 'NONE',  ( 7.027753727702739539, 7.098671581784288698, 19.74886208192143044 ) ) ;
#5044 = CARTESIAN_POINT ( 'NONE',  ( -4.579542530753125895, 8.877401133907090625, 7.148862081921437017 ) ) ;
#5045 = CARTESIAN_POINT ( 'NONE',  ( -13.61519076058348254, -8.404922754268771001, 8.718326283912148256 ) ) ;
#5046 = CARTESIAN_POINT ( 'NONE',  ( -11.60466159355861926, -11.60466159355875249, 28.50000000000001066 ) ) ;
#5047 = DIRECTION ( 'NONE',  ( 0.000000000000000000, 8.191099868251448390E-34, 1.000000000000000000 ) ) ;
#5048 = CARTESIAN_POINT ( 'NONE',  ( -8.620103694221995738, -13.47998361472161299, 2.289754855340722539 ) ) ;
#5049 = CARTESIAN_POINT ( 'NONE',  ( -11.85413878919593422, -7.448449071214776396, 16.71428571428571530 ) ) ;
#5050 = FACE_OUTER_BOUND ( 'NONE', #2393, .T. ) ;
#5051 = CARTESIAN_POINT ( 'NONE',  ( -1.689666864740335228, 10.36326688006722740, 4.298862081921427603 ) ) ;
#5052 = EDGE_LOOP ( 'NONE', ( #774, #1329, #9468, #3141 ) ) ;
#5053 = CARTESIAN_POINT ( 'NONE',  ( -7.639999817571787588, 12.15899005565156266, 18.21428571428571885 ) ) ;
#5054 = ORIENTED_EDGE ( 'NONE', *, *, #1535, .F. ) ;
#5055 = CARTESIAN_POINT ( 'NONE',  ( -5.420364854931998266, -15.49051278174643898, 34.07142857142857650 ) ) ;
#5056 = CARTESIAN_POINT ( 'NONE',  ( 11.40355824106246985, -11.22385875690704538, 46.99595943037356705 ) ) ;
#5057 = CARTESIAN_POINT ( 'NONE',  ( -7.424621202458789426, 7.424621202458724589, 6.000000000000005329 ) ) ;
#5058 = CARTESIAN_POINT ( 'NONE',  ( -7.639999817571786700, 12.15899005565156266, 6.214285714285717077 ) ) ;
#5059 = CARTESIAN_POINT ( 'NONE',  ( 1.737328882695370558, -14.25515036105620581, 23.63881657323070939 ) ) ;
#5060 = ORIENTED_EDGE ( 'NONE', *, *, #5467, .T. ) ;
#5061 = DIRECTION ( 'NONE',  ( 0.000000000000000000, 6.938893903907221444E-18, 1.000000000000000000 ) ) ;
#5062 = DIRECTION ( 'NONE',  ( 0.000000000000000000, 0.000000000000000000, 1.000000000000000000 ) ) ;
#5063 = CARTESIAN_POINT ( 'NONE',  ( 4.619798703721856192, 13.59724543428036725, 33.06738800180213644 ) ) ;
#5064 = CARTESIAN_POINT ( 'NONE',  ( 1.595456901104624459, -10.37818827243065201, 12.80113791807860224 ) ) ;
#5065 = CARTESIAN_POINT ( 'NONE',  ( -4.967534682030703586, 9.859792900771061852, 2.151137918078574796 ) ) ;
#5066 = CARTESIAN_POINT ( 'NONE',  ( -163.3500000000000512, -1.734723475976807094E-15, 3.000000000000002665 ) ) ;
#5067 = CARTESIAN_POINT ( 'NONE',  ( -9.809645194534070356, 9.989344678689256796, 16.00404056962643651 ) ) ;
#5068 = CARTESIAN_POINT ( 'NONE',  ( -10.24623928997352351, -10.06191849875416899, 26.50404056962643651 ) ) ;
#5069 = CARTESIAN_POINT ( 'NONE',  ( 10.37072757624895836, -1.642561882922355609, 10.19999999999998685 ) ) ;
#5070 = CARTESIAN_POINT ( 'NONE',  ( 15.14410076328353227, -5.164528828830166063, 34.56738800180213644 ) ) ;
#5071 = CARTESIAN_POINT ( 'NONE',  ( -12.72000065966944504, 8.744481972363274735, 48.72999999999997556 ) ) ;
#5072 = CARTESIAN_POINT ( 'NONE',  ( 13.89598863503046111, -8.731428362939032795, 20.78571428571429180 ) ) ;
#5073 = CARTESIAN_POINT ( 'NONE',  ( -1.665163862719845067, -15.91362231745477374, 11.85310228751642470 ) ) ;
#5074 = FACE_BOUND ( 'NONE', #4387, .T. ) ;
#5075 =( GEOMETRIC_REPRESENTATION_CONTEXT ( 3 ) GLOBAL_UNCERTAINTY_ASSIGNED_CONTEXT ( ( #5958 ) ) GLOBAL_UNIT_ASSIGNED_CONTEXT ( ( #1611, #2430, #3155 ) ) REPRESENTATION_CONTEXT ( 'NONE', 'WORKASPACE' ) );
#5076 = CARTESIAN_POINT ( 'NONE',  ( -4.490180821391513533, 8.922933199037158758, 2.151137918078574796 ) ) ;
#5077 = CARTESIAN_POINT ( 'NONE',  ( 9.865911304835474738, 1.562606840307950051, 13.04999999999999538 ) ) ;
#5078 = CARTESIAN_POINT ( 'NONE',  ( -166.0822128819447698, 1.878756849882351254, 14.88227075829311552 ) ) ;
#5079 = CARTESIAN_POINT ( 'NONE',  ( 4.742819248065503146, 13.55419868402813677, 37.07142857142857650 ) ) ;
#5080 = CARTESIAN_POINT ( 'NONE',  ( 10.15407889436379030, 10.15407889436390576, 37.50000000000002842 ) ) ;
#5081 = VERTEX_POINT ( 'NONE', #8659 ) ;
#5082 = AXIS2_PLACEMENT_3D ( 'NONE', #3767, #9201, #6734 ) ;
#5083 = CARTESIAN_POINT ( 'NONE',  ( 8.512513224245308763, 13.54758718765259040, 49.28571428571428470 ) ) ;
#5084 = FACE_OUTER_BOUND ( 'NONE', #9517, .T. ) ;
#5085 = CARTESIAN_POINT ( 'NONE',  ( 16.30827793483735633, -1.837501619626142890, 14.35714285714285587 ) ) ;
#5086 =( LENGTH_UNIT ( ) NAMED_UNIT ( * ) SI_UNIT ( .MILLI., .METRE. ) );
#5087 = PRODUCT ( 'base support', 'base support', '', ( #10170 ) ) ;
#5088 = B_SPLINE_CURVE_WITH_KNOTS ( 'NONE', 3,
 ( #7291, #106, #8802, #1720, #6351, #214, #2482, #5636, #4866, #4815, #3411, #6547, #1866, #5014, #838, #943, #4089, #9529, #2435, #5581, #7965, #1288, #7387, #4337, #7440, #9104, #2014, #8265, #1188, #416 ),
 .UNSPECIFIED., .F., .F.,
 ( 4, 2, 2, 2, 2, 2, 2, 2, 2, 2, 2, 2, 2, 2, 4 ),
 ( 6.815973429434667561E-18, 0.0003227411465790211431, 0.0006454822931580354558, 0.0009682234397370497684, 0.001290964586316063973, 0.001936446879474092598, 0.002581929172632121440, 0.002904670319211177278, 0.003227411465790232682, 0.003550152612369288519, 0.003872893758948343923, 0.004195634905527399761, 0.004518376052106455598, 0.004841117198685510568, 0.005163858345264566406 ),
 .UNSPECIFIED. ) ;
#5089 = FACE_OUTER_BOUND ( 'NONE', #467, .T. ) ;
#5090 = CARTESIAN_POINT ( 'NONE',  ( -6.717514421272238856, 6.717514421272181124, 0.000000000000000000 ) ) ;
#5091 = CARTESIAN_POINT ( 'NONE',  ( 8.442910196168311288, 4.355403765523574222, 10.89886208192140771 ) ) ;
#5092 = CARTESIAN_POINT ( 'NONE',  ( -11.22385875690717327, 11.40355824106234550, 16.00404056962643651 ) ) ;
#5093 = CARTESIAN_POINT ( 'NONE',  ( -13.54758718765249625, -8.512513224245459753, 34.71428571428571530 ) ) ;
#5094 = DIRECTION ( 'NONE',  ( 0.000000000000000000, 1.387778780781445676E-16, -1.000000000000000000 ) ) ;
#5095 = CARTESIAN_POINT ( 'NONE',  ( -13.61519076058348254, -8.404922754268771001, 8.718326283912148256 ) ) ;
#5096 = CARTESIAN_POINT ( 'NONE',  ( 7.639999817571789364, -12.15899005565156266, 21.21428571428571885 ) ) ;
#5097 = CARTESIAN_POINT ( 'NONE',  ( -16.30827793483735988, 1.837501619626141780, 11.35714285714285943 ) ) ;
#5098 = DIRECTION ( 'NONE',  ( 1.540743955509788409E-32, 0.8660254037844380415, -0.5000000000000012212 ) ) ;
#5099 = ORIENTED_EDGE ( 'NONE', *, *, #8480, .T. ) ;
#5100 = CARTESIAN_POINT ( 'NONE',  ( 13.55419868402807992, 4.742819248065648807, 19.92857142857143771 ) ) ;
#5101 = ORIENTED_EDGE ( 'NONE', *, *, #6228, .T. ) ;
#5102 = CARTESIAN_POINT ( 'NONE',  ( 8.731428362939189114, -13.89598863503035986, 33.21428571428571530 ) ) ;
#5103 = CARTESIAN_POINT ( 'NONE',  ( -12.22833218042443271, 7.529642458189139909, 7.781673716087849968 ) ) ;
#5104 = CARTESIAN_POINT ( 'NONE',  ( -10.37072757624895836, 1.642561882922380034, 14.69999999999999041 ) ) ;
#5105 =( NAMED_UNIT ( * ) SI_UNIT ( $, .STERADIAN. ) SOLID_ANGLE_UNIT ( ) );
#5106 = CARTESIAN_POINT ( 'NONE',  ( 13.21436662431716869, -4.623906867372263640, 8.571428571428569398 ) ) ;
#5107 = VERTEX_POINT ( 'NONE', #2397 ) ;
#5108 = CARTESIAN_POINT ( 'NONE',  ( -10.06191849875405531, -10.24623928997363542, 24.49595943037356705 ) ) ;
#5109 = VERTEX_POINT ( 'NONE', #800 ) ;
#5110 =( LENGTH_UNIT ( ) NAMED_UNIT ( * ) SI_UNIT ( .MILLI., .METRE. ) );
#5111 = DIRECTION ( 'NONE',  ( 0.000000000000000000, -6.338944243255235518E-49, 1.000000000000000000 ) ) ;
#5112 = CARTESIAN_POINT ( 'NONE',  ( -1.689666864740335228, 10.36326688006723451, 16.29886208192143471 ) ) ;
#5113 = CARTESIAN_POINT ( 'NONE',  ( 13.55419868402807992, 4.742819248065648807, 1.928571428571430380 ) ) ;
#5114 = CARTESIAN_POINT ( 'NONE',  ( 4.766900247265192903, 9.355568503977902850, 3.599999999999992095 ) ) ;
#5115 = CARTESIAN_POINT ( 'NONE',  ( -7.842167650704559456, -7.771249796623180828, 4.251137918078595312 ) ) ;
#5116 = CARTESIAN_POINT ( 'NONE',  ( -165.0000000000000284, -1.734723475976807094E-15, 3.000000000000002665 ) ) ;
#5117 = CARTESIAN_POINT ( 'NONE',  ( 7.556039541191335474, 11.78653521626503320, 35.28975485534072476 ) ) ;
#5118 = AXIS2_PLACEMENT_3D ( 'NONE', #9417, #7073, #9316 ) ;
#5119 = AXIS2_PLACEMENT_3D ( 'NONE', #6365, #4984, #5698 ) ;
#5120 =( NAMED_UNIT ( * ) PLANE_ANGLE_UNIT ( ) SI_UNIT ( $, .RADIAN. ) );
#5121 = CARTESIAN_POINT ( 'NONE',  ( -1.478298951650703019, 14.28433602490913579, 28.64689771248357886 ) ) ;
#5122 = EDGE_CURVE ( 'NONE', #999, #1541, #4020, .T. ) ;
#5123 = CARTESIAN_POINT ( 'NONE',  ( -5.012215536711506658, 9.837026868206027785, 3.149999999999957723 ) ) ;
#5124 = CARTESIAN_POINT ( 'NONE',  ( 15.88516839912898071, 1.917699372586004092, 34.13881657323070584 ) ) ;
#5125 = CARTESIAN_POINT ( 'NONE',  ( -13.17294599347781769, 7.596107530180142398, 48.73000000000000398 ) ) ;
#5126 = CARTESIAN_POINT ( 'NONE',  ( -8.731428362939189114, 13.89598863503036341, 24.21428571428571530 ) ) ;
#5127 = ADVANCED_FACE ( 'NONE', ( #3853 ), #4677, .F. ) ;
#5128 = LINE ( 'NONE', #2077, #402 ) ;
#5129 = CONICAL_SURFACE ( 'NONE', #3977, 1.649999999999984812, 1.029744258676650093 ) ;
#5130 = CIRCLE ( 'NONE', #4137, 18.00000000000000355 ) ;
#5131 = VECTOR ( 'NONE', #3101, 1000.000000000000000 ) ;
#5132 = ADVANCED_FACE ( 'NONE', ( #9492 ), #1427, .F. ) ;
#5133 = CARTESIAN_POINT ( 'NONE',  ( 13.25633410266679313, -4.503970704919842305, 10.56738800180213644 ) ) ;
#5134 = CARTESIAN_POINT ( 'NONE',  ( 7.098671581784200768, 7.027753727702831021, 2.751137918078555789 ) ) ;
#5135 = CARTESIAN_POINT ( 'NONE',  ( -7.063212654743466601, -7.063212654743531438, 17.25000000000003553 ) ) ;
#5136 = CARTESIAN_POINT ( 'NONE',  ( -68.00000000000002842, 2.204364238465235822E-15, -18.00000000000000355 ) ) ;
#5137 = CARTESIAN_POINT ( 'NONE',  ( -9.899494936611716867, 9.899494936611610285, 30.00000000000000355 ) ) ;
#5138 = PRESENTATION_LAYER_ASSIGNMENT (  '', '', ( #4486 ) ) ;
#5139 = CARTESIAN_POINT ( 'NONE',  ( 9.899494936611718643, -9.899494936611608509, 33.00000000000000000 ) ) ;
#5140 = ORIENTED_EDGE ( 'NONE', *, *, #2171, .T. ) ;
#5141 = CARTESIAN_POINT ( 'NONE',  ( -8.731428362939189114, 13.89598863503036341, 48.21428571428570820 ) ) ;
#5142 = DIRECTION ( 'NONE',  ( 1.000000000000000000, 4.755747939841215952E-17, -0.000000000000000000 ) ) ;
#5143 = CARTESIAN_POINT ( 'NONE',  ( 5.420364854932001819, 15.49051278174644430, 19.07142857142856940 ) ) ;
#5144 = DIRECTION ( 'NONE',  ( -0.000000000000000000, -0.000000000000000000, 1.000000000000000000 ) ) ;
#5145 = CARTESIAN_POINT ( 'NONE',  ( -9.390499931835536884, 1.439022436064298249, 18.69886208192145816 ) ) ;
#5146 = CARTESIAN_POINT ( 'NONE',  ( 4.579542530753127672, -8.877401133907065756, 5.648862081921440570 ) ) ;
#5147 = UNCERTAINTY_MEASURE_WITH_UNIT (LENGTH_MEASURE( 1.000000000000000082E-05 ), #113, 'distance_accuracy_value', 'NONE');
#5148 = CARTESIAN_POINT ( 'NONE',  ( 1.727091770866550968, 10.90442828429187294, 12.44999999999995666 ) ) ;
#5149 = CARTESIAN_POINT ( 'NONE',  ( 11.69682198916835070, 11.51250119794901394, 11.50404056962644006 ) ) ;
#5150 = CARTESIAN_POINT ( 'NONE',  ( 13.89598863503046111, -8.731428362939032795, 26.78571428571429536 ) ) ;
#5151 = FACE_OUTER_BOUND ( 'NONE', #9603, .T. ) ;
#5152 = CARTESIAN_POINT ( 'NONE',  ( 16.29368510291089223, -1.967016585148476882, 12.36118342676929771 ) ) ;
#5153 = CARTESIAN_POINT ( 'NONE',  ( -4.623906867372410190, 13.21436662431711895, 30.42857142857143060 ) ) ;
#5154 = ADVANCED_FACE ( 'NONE', ( #5546, #3800 ), #3901, .T. ) ;
#5155 = CARTESIAN_POINT ( 'NONE',  ( 15.10213328493390783, -5.284464991282587398, 2.571428571428571619 ) ) ;
#5156 = CARTESIAN_POINT ( 'NONE',  ( 1.791431617652837316, 15.89939535829188877, 42.85714285714285410 ) ) ;
#5157 = ORIENTED_EDGE ( 'NONE', *, *, #8032, .F. ) ;
#5158 = CARTESIAN_POINT ( 'NONE',  ( 12.15899005565164792, -7.639999817571655250, 20.78571428571429180 ) ) ;
#5159 = ORIENTED_EDGE ( 'NONE', *, *, #310, .F. ) ;
#5160 = CARTESIAN_POINT ( 'NONE',  ( 5.284464991282756152, -15.10213328493384743, 27.42857142857143060 ) ) ;
#5161 = CARTESIAN_POINT ( 'NONE',  ( 11.78653521626494793, 7.556039541191463371, 3.710245144659281458 ) ) ;
#5162 = CARTESIAN_POINT ( 'NONE',  ( -1.689666864740335228, 10.36326688006723273, 1.298862081921425604 ) ) ;
#5163 =( NAMED_UNIT ( * ) PLANE_ANGLE_UNIT ( ) SI_UNIT ( $, .RADIAN. ) );
#5164 = CARTESIAN_POINT ( 'NONE',  ( -4.742819248065500481, -13.55419868402813499, 16.07142857142857650 ) ) ;
#5165 = EDGE_CURVE ( 'NONE', #7090, #3093, #8606, .T. ) ;
#5166 = CARTESIAN_POINT ( 'NONE',  ( 11.78653521626494793, 7.556039541191463371, 27.71024514465928235 ) ) ;
#5167 = ORIENTED_EDGE ( 'NONE', *, *, #8383, .T. ) ;
#5168 = CARTESIAN_POINT ( 'NONE',  ( 9.837026868206070418, -5.012215536711392083, 19.34999999999997300 ) ) ;
#5169 = ADVANCED_FACE ( 'NONE', ( #7045, #7921, #4006 ), #3224, .T. ) ;
#5170 = CARTESIAN_POINT ( 'NONE',  ( -9.899494936611716867, 9.899494936611610285, 0.000000000000000000 ) ) ;
#5171 = CARTESIAN_POINT ( 'NONE',  ( 4.579542530753127672, -8.877401133907065756, 2.648862081921448119 ) ) ;
#5172 = CARTESIAN_POINT ( 'NONE',  ( 7.639999817571789364, -12.15899005565156266, 3.214285714285716633 ) ) ;
#5173 = CARTESIAN_POINT ( 'NONE',  ( -10.37072757624895836, 1.642561882922380923, 2.699999999999980194 ) ) ;
#5174 = CARTESIAN_POINT ( 'NONE',  ( 4.809394265263009061, 9.333916720356734587, 2.601137918078560762 ) ) ;
#5175 = CARTESIAN_POINT ( 'NONE',  ( 6.976602070941136269, -13.58603705635637304, -1.270000000000007123 ) ) ;
#5176 = CARTESIAN_POINT ( 'NONE',  ( 13.59724543428031573, 4.619798703722006294, 29.93261199819786356 ) ) ;
#5177 = PRODUCT_DEFINITION_SHAPE ( 'NONE', 'NONE',  #9415 ) ;
#5178 = CARTESIAN_POINT ( 'NONE',  ( 9.355568503977840678, 4.766900247265305701, 6.899999999999961275 ) ) ;
#5179 = CARTESIAN_POINT ( 'NONE',  ( -16.32287076676382398, 1.707986654103809343, 37.35310228751641404 ) ) ;
#5180 = CARTESIAN_POINT ( 'NONE',  ( -68.00000000000002842, 0.000000000000000000, 0.000000000000000000 ) ) ;
#5181 = DIRECTION ( 'NONE',  ( 0.000000000000000000, 0.000000000000000000, 1.000000000000000000 ) ) ;
#5182 = CARTESIAN_POINT ( 'NONE',  ( 4.619798703721856192, 13.59724543428036725, 15.06738800180213822 ) ) ;
#5183 = CARTESIAN_POINT ( 'NONE',  ( 8.486213763410640709, 4.270415729527937465, 14.90113791807857879 ) ) ;
#5184 = CARTESIAN_POINT ( 'NONE',  ( 6.717514421272239744, -6.717514421272154479, 13.50000000000001243 ) ) ;
#5185 = CARTESIAN_POINT ( 'NONE',  ( -167.1360214673730979, 0.2820915794957485345, 14.99797831373487078 ) ) ;
#5186 = CARTESIAN_POINT ( 'NONE',  ( 13.21436662431716869, -4.623906867372263640, 38.57142857142857650 ) ) ;
#5187 = ADVANCED_FACE ( 'NONE', ( #9337 ), #1027, .F. ) ;
#5188 = CARTESIAN_POINT ( 'NONE',  ( 4.742819248065503146, 13.55419868402813677, 37.07142857142857650 ) ) ;
#5189 = ORIENTED_EDGE ( 'NONE', *, *, #6503, .F. ) ;
#5190 = CARTESIAN_POINT ( 'NONE',  ( -15.10213328493390961, 5.284464991282586510, 47.57142857142857650 ) ) ;
#5191 = CARTESIAN_POINT ( 'NONE',  ( 0.000000000000000000, 0.000000000000000000, 0.000000000000000000 ) ) ;
#5192 = CARTESIAN_POINT ( 'NONE',  ( 15.10213328493390783, -5.284464991282587398, 32.57142857142856940 ) ) ;
#5193 = CARTESIAN_POINT ( 'NONE',  ( -68.00000000000002842, 2.204364238465235822E-15, -18.00000000000000355 ) ) ;
#5194 = PRESENTATION_STYLE_ASSIGNMENT (( #7683 ) ) ;
#5195 = CARTESIAN_POINT ( 'NONE',  ( -55.00000000000002132, 7.703719777548943412E-30, -7.703719777548943412E-31 ) ) ;
#5196 = CARTESIAN_POINT ( 'NONE',  ( -1.486127417882243895, 9.383039235653825472, 6.299999999999972289 ) ) ;
#5197 = CARTESIAN_POINT ( 'NONE',  ( -4.579542530753125895, 8.877401133907083519, 4.148862081921444123 ) ) ;
#5198 = CARTESIAN_POINT ( 'NONE',  ( -9.837026868206066865, 5.012215536711413399, 14.84999999999999787 ) ) ;
#5199 = CARTESIAN_POINT ( 'NONE',  ( 13.82664651025767100, -8.841785722321541030, 12.78975485534072121 ) ) ;
#5200 = CARTESIAN_POINT ( 'NONE',  ( -5.420364854931999155, -15.49051278174644253, 40.07142857142857650 ) ) ;
#5201 = PRESENTATION_STYLE_ASSIGNMENT (( #2151 ) ) ;
#5202 = CARTESIAN_POINT ( 'NONE',  ( 15.53355953199861794, 5.297344310588528060, 5.932611998197868886 ) ) ;
#5203 = CARTESIAN_POINT ( 'NONE',  ( -1.791431617652833763, -15.89939535829188877, 3.857142857142857650 ) ) ;
#5204 = CARTESIAN_POINT ( 'NONE',  ( 13.89598863503046111, -8.731428362939032795, 44.78571428571428470 ) ) ;
#5205 = ORIENTED_EDGE ( 'NONE', *, *, #1300, .T. ) ;
#5206 = CARTESIAN_POINT ( 'NONE',  ( -9.837026868206066865, 5.012215536711416064, 17.85000000000001918 ) ) ;
#5207 = ORIENTED_EDGE ( 'NONE', *, *, #7105, .F. ) ;
#5208 = CARTESIAN_POINT ( 'NONE',  ( -1.837501619626327853, 16.30827793483733856, 24.64285714285714235 ) ) ;
#5209 = CARTESIAN_POINT ( 'NONE',  ( 1.441234910513245149, 13.92619789766829008, 2.853102287516426916 ) ) ;
#5210 = CARTESIAN_POINT ( 'NONE',  ( -4.766900247265192014, -9.355568503977876205, 17.10000000000000497 ) ) ;
#5211 = APPLICATION_PROTOCOL_DEFINITION ( 'draft international standard', 'automotive_design', 1998, #7509 ) ;
#5212 = CARTESIAN_POINT ( 'NONE',  ( 7.639999817571788476, -12.15899005565156266, 27.21428571428571885 ) ) ;
#5213 = ORIENTED_EDGE ( 'NONE', *, *, #4948, .T. ) ;
#5214 = CARTESIAN_POINT ( 'NONE',  ( -14.28433602490915000, 1.478298951650542481, 31.35310228751642470 ) ) ;
#5215 = VERTEX_POINT ( 'NONE', #8552 ) ;
#5216 = PLANE ( 'NONE',  #1563 ) ;
#5217 = CARTESIAN_POINT ( 'NONE',  ( -9.859792900771106261, 4.967534682030611215, 18.84886208192146029 ) ) ;
#5218 = CARTESIAN_POINT ( 'NONE',  ( -9.355568503977838901, -4.766900247265279944, 5.400000000000016342 ) ) ;
#5219 = CARTESIAN_POINT ( 'NONE',  ( 1.776620879821457333, 10.89658364409028124, 11.45113791807854220 ) ) ;
#5220 = CARTESIAN_POINT ( 'NONE',  ( -58.00000000000001421, 0.000000000000000000, 0.000000000000000000 ) ) ;
#5221 = CARTESIAN_POINT ( 'NONE',  ( -1.693770420379220099, -13.89774397934251837, 25.86118342676929416 ) ) ;
#5222 = CARTESIAN_POINT ( 'NONE',  ( 10.37072757624895836, -1.642561882922355609, 4.199999999999981526 ) ) ;
#5223 = CARTESIAN_POINT ( 'NONE',  ( 1.967016585148662289, -16.29368510291087091, 35.63881657323071295 ) ) ;
#5224 = CARTESIAN_POINT ( 'NONE',  ( -13.04911192085559790, 7.214667598204639987, 48.73000000000001819 ) ) ;
#5225 = DIRECTION ( 'NONE',  ( -1.000000000000000000, 1.842239752758738928E-31, -1.780435181894459419E-32 ) ) ;
#5226 = CARTESIAN_POINT ( 'NONE',  ( -13.51115193377584589, -4.865839792409295761, 18.92453085894499409 ) ) ;
#5227 = CARTESIAN_POINT ( 'NONE',  ( 7.098671581784200768, 7.027753727702831021, 17.75113791807856245 ) ) ;
#5228 = CARTESIAN_POINT ( 'NONE',  ( 4.355403765523470305, 8.442910196168364578, 2.601137918078560762 ) ) ;
#5229 = CARTESIAN_POINT ( 'NONE',  ( -163.1351247077966491, 1.079043896566285632, 14.96159378939550599 ) ) ;
#5230 = CARTESIAN_POINT ( 'NONE',  ( 13.21436662431716869, -4.623906867372263640, 44.57142857142857650 ) ) ;
#5231 = CARTESIAN_POINT ( 'NONE',  ( 7.556039541191335474, 11.78653521626503320, 5.289754855340725648 ) ) ;
#5232 = VERTEX_POINT ( 'NONE', #3271 ) ;
#5233 = CARTESIAN_POINT ( 'NONE',  ( -1.837501619626328297, 16.30827793483733856, 42.64285714285715301 ) ) ;
#5234 = CARTESIAN_POINT ( 'NONE',  ( 13.61000000000001720, 0.000000000000000000, 0.000000000000000000 ) ) ;
#5235 = CARTESIAN_POINT ( 'NONE',  ( -1.837501619626328297, 16.30827793483733856, 30.64285714285715301 ) ) ;
#5236 = CYLINDRICAL_SURFACE ( 'NONE', #4496, 15.44569104238500046 ) ;
#5237 = DIRECTION ( 'NONE',  ( -1.000000000000000000, -0.000000000000000000, -0.000000000000000000 ) ) ;
#5238 = PLANE ( 'NONE',  #1671 ) ;
#5239 = CARTESIAN_POINT ( 'NONE',  ( -9.383039235653820143, 1.486127417882155521, 8.700000000000041922 ) ) ;
#5240 = CARTESIAN_POINT ( 'NONE',  ( -9.858066664633883036, -1.612135949262833101, 12.54886208192144004 ) ) ;
#5241 = CARTESIAN_POINT ( 'NONE',  ( -9.355568503977838901, -4.766900247265279944, 11.39999999999996660 ) ) ;
#5242 = CARTESIAN_POINT ( 'NONE',  ( 1.837501619626330074, -16.30827793483733501, 39.64285714285716722 ) ) ;
#5243 = CARTESIAN_POINT ( 'NONE',  ( 13.82664651025767100, -8.841785722321541030, 24.78975485534072476 ) ) ;
#5244 = CARTESIAN_POINT ( 'NONE',  ( 1.567502665446232957, 13.91197093850540156, 24.85714285714285765 ) ) ;
#5245 = DIRECTION ( 'NONE',  ( 0.000000000000000000, 8.191099868251446680E-34, 1.000000000000000000 ) ) ;
#5246 = CARTESIAN_POINT ( 'NONE',  ( -15.10213328493390961, 5.284464991282586510, 41.57142857142856940 ) ) ;
#5247 = ORIENTED_EDGE ( 'NONE', *, *, #2743, .F. ) ;
#5248 = CARTESIAN_POINT ( 'NONE',  ( 1.727091770866550968, 10.90442828429187294, 12.44999999999995666 ) ) ;
#5249 = CARTESIAN_POINT ( 'NONE',  ( -158.0000000000000284, -6.938893903907228378E-15, 0.000000000000000000 ) ) ;
#5250 = CARTESIAN_POINT ( 'NONE',  ( -160.0000000000000284, 14.99999999999999289, 0.000000000000000000 ) ) ;
#5251 = CARTESIAN_POINT ( 'NONE',  ( 1.737328882695370558, -14.25515036105620581, 5.638816573230711171 ) ) ;
#5252 = CARTESIAN_POINT ( 'NONE',  ( 7.424621202458790314, -7.424621202458697944, 13.50000000000001243 ) ) ;
#5253 = CARTESIAN_POINT ( 'NONE',  ( 15.89939535829187278, 1.791431617653015174, 8.142857142857145902 ) ) ;
#5254 = CARTESIAN_POINT ( 'NONE',  ( 5.420364854932001819, 15.49051278174644430, 7.071428571428569398 ) ) ;
#5255 = CARTESIAN_POINT ( 'NONE',  ( -7.639999817571786700, 12.15899005565156266, 24.21428571428571530 ) ) ;
#5256 = CARTESIAN_POINT ( 'NONE',  ( 13.51115193377584589, 4.865839792409294873, 39.92453085894499054 ) ) ;
#5257 = ORIENTED_EDGE ( 'NONE', *, *, #4861, .F. ) ;
#5258 = FACE_OUTER_BOUND ( 'NONE', #9916, .T. ) ;
#5259 = CARTESIAN_POINT ( 'NONE',  ( -5.404401153735176599, 15.06016580658422477, 20.42453085894499054 ) ) ;
#5260 = CARTESIAN_POINT ( 'NONE',  ( -13.54758718765249625, -8.512513224245459753, 10.71428571428571708 ) ) ;
#5261 = CARTESIAN_POINT ( 'NONE',  ( -10.89658364409024749, -1.776620879821559917, 18.54886208192142405 ) ) ;
#5262 = CARTESIAN_POINT ( 'NONE',  ( 10.90442828429183919, 1.727091770866679532, 10.05000000000002736 ) ) ;
#5263 = CARTESIAN_POINT ( 'NONE',  ( -10.36326688006724162, 1.689666864740235308, 16.70113791807854398 ) ) ;
#5264 = CARTESIAN_POINT ( 'NONE',  ( 2.000000000000001776, -0.8865213383406761460, 1.535499999999911935 ) ) ;
#5265 = CARTESIAN_POINT ( 'NONE',  ( -4.503970704919988854, 13.25633410266674517, 34.43261199819786356 ) ) ;
#5266 = VECTOR ( 'NONE', #7785, 1000.000000000000227 ) ;
#5267 =( BOUNDED_SURFACE ( )  B_SPLINE_SURFACE ( 3, 2, ( 
 ( #828, #3832, #5478, #3048, #734, #7903, #2376, #5527, #6190, #4706, #8686, #1608, #7133, #9365, #3207, #6341, #2277, #5424, #8736, #1656, #8581, #779, #3882, #9521, #5573, #7381, #4858, #3448, #8847, #1804, #1135, #4959, #1908, #2624, #8111, #8054, #2581, #4230, #209, #4184, #5057, #2529, #5770, #5009, #5724, #1858, #1757, #8155, #1089, #5678, #7285, #7334, #307, #4908, #150, #6590, #984, #4133, #6541, #5822, #1040, #6494, #3359, #9672, #8892, #9773, #2676, #258, #3405, #8999, #8203, #4280, #5627, #9720, #8945, #7432, #3252, #6392, #9570, #2473, #8793, #1713, #8005, #935, #6446, #4080, #7230, #3305, #9626, #9867, #5252, #4545, #4384, #2166, #9095, #9199, #1281, #510, #5104, #5972, #9970, #2878, #7585, #9246, #8408, #3656, #6683, #9822, #2928, #8313, #361, #3508, #6845, #1233, #5210, #8256, #6638, #4439, #411, #2724, #6793, #7643, #563, #7535, #4489, #3711, #1183, #5310, #4332, #1335, #7483 ),
 ( #6020, #462, #5162, #10016, #2008, #5919, #2109, #6071, #8467, #3555, #1392, #5867, #8360, #3601, #6733, #9924, #2827, #9045, #1955, #9150, #2772, #2057, #3191, #5514, #10065, #6175, #5463, #9402, #8567, #2414, #5560, #7799, #1593, #3866, #8674, #617, #667, #814, #4743, #2313, #1490, #6955, #2361, #1643, #4644, #9508, #9351, #6276, #8624, #7839, #2216, #3083, #7058, #10220, #4693, #6327, #7889, #766, #3820, #6898, #34, #5409, #7698, #3764, #3967, #720, #1545, #5362, #2982, #3912, #7747, #6128, #3131, #7118, #8721, #7009, #9302, #8518, #1442, #4593, #10119, #3034, #2261, #6226, #10167, #9459, #6377, #9556, #7166, #4022, #2461, #84, #3239, #5609, #8779, #4787, #870, #7942, #1289, #6857, #2939, #6740, #5112, #4287, #2887, #8421, #5876, #4503, #9876, #2836, #2181, #5980, #6082, #3668, #9159, #9106, #3610, #5261, #1239, #5217, #9259, #3561, #6803, #6029, #9932, #9209, #2780, #2120, #1348, #6692, #8321 ),
 ( #7656, #575, #3720, #4393, #9054, #10029, #5324, #6645, #5928, #2066, #8369, #5171, #8479, #7441, #7543, #367, #469, #3517, #9830, #7492, #2730, #1963, #4445, #7596, #2015, #8266, #1189, #521, #4339, #9980, #418, #2459, #1696, #6138, #7023, #918, #134, #8774, #190, #6427, #4840, #681, #629, #4117, #9363, #1404, #4557, #8039, #2275, #6237, #9314, #7708, #5607, #4605, #3777, #7991, #8830, #1741, #8579, #5662, #4892, #2227, #6477, #5373, #9609, #8529, #10181, #2513, #968, #3285, #7263, #5422, #6187, #3343, #10130, #6968, #6909, #10079, #2995, #3830, #3046, #732, #3880, #3097, #9414, #9702, #8875, #7468, #2756, #240, #9079, #4214, #7414, #6719, #342, #7520, #8238, #3492, #3435, #8188, #9852, #5807, #9807, #444, #8138, #1166, #396, #1120, #3542, #7366, #6668, #5904, #1074, #2660, #2709, #1990, #292, #5754, #5145, #6572, #9755, #1940, #1217, #6622, #1894, #5043, #4266, #5852, #8296, #4368, #9029 ),
 ( #5090, #4994, #4318, #3585, #9903, #2810, #1790, #4169, #4941, #8090, #1019, #2609, #7317, #3390, #6524, #8923, #1840, #5293, #6773, #4421, #7571, #8450, #4579, #1377, #9340, #6996, #9290, #2911, #10109, #3803, #547, #10156, #6055, #8503, #5956, #6164, #9958, #492, #3021, #2090, #9230, #4628, #5196, #2861, #9185, #2039, #9136, #8344, #7786, #8393, #708, #5396, #3638, #1318, #6007, #2249, #6939, #2146, #5239, #8554, #1480, #3855, #4528, #4472, #7685, #7628, #7736, #654, #3695, #1263, #6829, #10003, #601, #3747, #6883, #10052, #2964, #6112, #2203, #5351, #1429, #1531, #4729, #4106, #7875, #802, #3950, #6213, #855, #5447, #1684, #4680, #4827, #2448, #23, #7980, #7096, #9593, #1732, #8025, #6260, #4055, #5548, #1629, #5501, #8818, #6313, #7828, #8707, #2500, #2351, #4007, #3273, #7154, #9494, #6414, #7925, #5594, #7202, #7047, #3177, #4776, #907, #121, #10206, #1581, #2399, #72, #3226, #6363, #5649 ),
 ( #4881, #956, #9541, #9445, #8757, #8608, #756, #3903, #7250, #3070, #9389, #2302, #3119, #8660, #8176, #2552, #9019, #1777, #1928, #9796, #7355, #5076, #1062, #6658, #9068, #5134, #3379, #1153, #2648, #8971, #2599, #5889, #3423, #4930, #5796, #9841, #9690, #1110, #381, #4254, #6561, #3533, #5031, #2700, #4304, #4155, #278, #1883, #8226, #7455, #7304, #8911, #8077, #1976, #6609, #6512, #7403, #2744, #8281, #1203, #4354, #5696, #173, #4203, #8864, #226, #5742, #3331, #9646, #327, #1827, #3476, #1007, #4982, #8128, #5841, #6468, #2898, #642, #8543, #588, #4456, #1418, #5337, #2079, #1466, #7613, #10039, #7506, #7722, #8332, #5943, #4568, #3621, #534, #6151, #6706, #1250, #479, #3572, #431, #9890, #9327, #9944, #2237, #6921, #5183, #2849, #7556, #3791, #8492, #3683, #9123, #10096, #3007, #5383, #6818, #2025, #4407, #2793, #4515, #6758, #5994, #9992, #9173, #5227, #6095, #8381, #1304, #6042, #9218 ),
 ( #6869, #2133, #5275, #8438, #1362, #7672, #3733, #2951, #9276, #2190, #6352, #3940, #3216, #3110, #9531, #2436, #7035, #8648, #8696, #5582, #6250, #1519, #8745, #9427, #10195, #7912, #7191, #2387, #7863, #2338, #1571, #790, #1668, #4817, #4717, #5537, #7967, #108, #897, #6981, #5490, #1618, #6301, #7084, #9579, #2484, #6, #4045, #3163, #3261, #7770, #7817, #6403, #5638, #9484, #4766, #3891, #8805, #4615, #839, #697, #3997, #3844, #7142, #60, #9376, #10143, #3057, #6201, #2290, #5433, #8592, #4666, #744, #946, #4288, #9681, #5878, #4869, #8212, #2588, #6549, #9635, #8014, #2633, #1765, #1723, #5781, #9005, #1916, #8900, #5829, #5064, #2539, #6647, #6456, #9785, #5685, #7343, #2686, #1142, #5016, #1868, #5733, #6501, #7443, #216, #7293, #8162, #3457, #370, #3367, #8855, #3519, #1097, #8065, #1814, #9832, #2732, #4092, #7241, #159, #3316, #4971, #4920, #993, #4142, #8120, #1050, #4194, #266 ),
 ( #3413, #316, #9732, #8956, #4238, #7389, #6599, #2941, #6858, #3611, #2997, #9161, #1350, #9056, #9261, #9878, #7494, #6084, #5173, #2068, #7710, #8268, #2782, #2016, #5114, #1964, #1191, #631, #1241, #3779, #8482, #6693, #4395, #9108, #2183, #5326, #5218, #420, #1406, #4559, #6911, #8370, #3563, #523, #5930, #7659, #577, #6742, #4341, #10081, #2838, #3722, #8323, #7544, #470, #7598, #9935, #5982, #1291, #4447, #3671, #6805, #9982, #2888, #6030, #9210, #2122, #5262, #8422, #4505, #4433, #1437, #2213, #10012, #4590, #3707, #9347, #1487, #7796, #6016, #3814, #5305, #1387, #5248, #8562, #6067, #7581, #8462, #2257, #2104, #3760, #3030, #6894, #9241, #6172, #7694, #5359, #6951, #6788, #2923, #4540, #7744, #10116, #9966, #2823, #9146, #4638, #8403, #717, #5405, #504, #1328, #2873, #3864, #7004, #2159, #1275, #5968, #2053, #5206, #613, #3651, #10062, #9195, #663, #8356, #558, #4484, #7639, #6840, #2975 ) ),
 .UNSPECIFIED., .T., .F., .F. ) 
 B_SPLINE_SURFACE_WITH_KNOTS ( ( 4, 3, 4 ),
 ( 3, 2, 2, 2, 2, 2, 2, 2, 2, 2, 2, 2, 2, 2, 2, 2, 2, 2, 2, 2, 2, 2, 2, 2, 2, 2, 2, 2, 2, 2, 2, 2, 2, 2, 2, 2, 2, 2, 2, 2, 2, 2, 2, 2, 2, 2, 2, 2, 2, 2, 2, 2, 2, 2, 2, 2, 2, 2, 2, 2, 2, 2, 2, 2, 2, 3 ),
 ( 0.000000000000000000, 0.5000000000000000000, 1.000000000000000000 ),
 ( 0.000000000000000000, 0.01428571428571428527, 0.02857142857142857054, 0.04285714285714285754, 0.05714285714285714107, 0.07142857142857142461, 0.08571428571428571508, 0.1000000000000000056, 0.1142857142857142821, 0.1285714285714285587, 0.1428571428571428492, 0.1571428571428571397, 0.1714285714285714302, 0.1857142857142857206, 0.2000000000000000111, 0.2142857142857142738, 0.2285714285714285643, 0.2428571428571428548, 0.2571428571428571175, 0.2714285714285714080, 0.2857142857142856984, 0.2999999999999999889, 0.3142857142857142794, 0.3285714285714285698, 0.3428571428571428603, 0.3571428571428571508, 0.3714285714285714413, 0.3857142857142857317, 0.4000000000000000222, 0.4142857142857143127, 0.4285714285714285476, 0.4428571428571428381, 0.4571428571428571286, 0.4714285714285714191, 0.4857142857142857095, 0.5000000000000000000, 0.5142857142857142350, 0.5285714285714285809, 0.5428571428571428159, 0.5571428571428571619, 0.5714285714285713969, 0.5857142857142857428, 0.5999999999999999778, 0.6142857142857143238, 0.6285714285714285587, 0.6428571428571429047, 0.6571428571428571397, 0.6714285714285713746, 0.6857142857142857206, 0.6999999999999999556, 0.7142857142857143016, 0.7285714285714285365, 0.7428571428571428825, 0.7571428571428571175, 0.7714285714285714635, 0.7857142857142856984, 0.8000000000000000444, 0.8142857142857142794, 0.8285714285714286254, 0.8428571428571428603, 0.8571428571428570953, 0.8714285714285714413, 0.8857142857142856762, 0.9000000000000000222, 0.9142857142857142572, 0.9285714285714286031 ),
 .UNSPECIFIED. ) 
 GEOMETRIC_REPRESENTATION_ITEM ( )  RATIONAL_B_SPLINE_SURFACE ( (
 ( 1.000000000000000000, 0.9510565162951535312, 1.000000000000000000, 0.9510565162951535312, 1.000000000000000000, 0.9510565162951535312, 1.000000000000000000, 0.9510565162951535312, 1.000000000000000000, 0.9510565162951535312, 1.000000000000000000, 0.9510565162951535312, 1.000000000000000000, 0.9510565162951535312, 1.000000000000000000, 0.9510565162951535312, 1.000000000000000000, 0.9510565162951535312, 1.000000000000000000, 0.9510565162951535312, 1.000000000000000000, 0.9510565162951535312, 1.000000000000000000, 0.9510565162951535312, 1.000000000000000000, 0.9510565162951535312, 1.000000000000000000, 0.9510565162951535312, 1.000000000000000000, 0.9510565162951535312, 1.000000000000000000, 0.9510565162951535312, 1.000000000000000000, 0.9510565162951535312, 1.000000000000000000, 0.9510565162951535312, 1.000000000000000000, 0.9510565162951535312, 1.000000000000000000, 0.9510565162951535312, 1.000000000000000000, 0.9510565162951535312, 1.000000000000000000, 0.9510565162951535312, 1.000000000000000000, 0.9510565162951535312, 1.000000000000000000, 0.9510565162951535312, 1.000000000000000000, 0.9510565162951535312, 1.000000000000000000, 0.9510565162951535312, 1.000000000000000000, 0.9510565162951535312, 1.000000000000000000, 0.9510565162951535312, 1.000000000000000000, 0.9510565162951535312, 1.000000000000000000, 0.9510565162951535312, 1.000000000000000000, 0.9510565162951535312, 1.000000000000000000, 0.9510565162951535312, 1.000000000000000000, 0.9510565162951535312, 1.000000000000000000, 0.9510565162951535312, 1.000000000000000000, 0.9510565162951535312, 1.000000000000000000, 0.9510565162951535312, 1.000000000000000000, 0.9510565162951535312, 1.000000000000000000, 0.9510565162951535312, 1.000000000000000000, 0.9510565162951535312, 1.000000000000000000, 0.9510565162951535312, 1.000000000000000000, 0.9510565162951535312, 1.000000000000000000, 0.9510565162951535312, 1.000000000000000000, 0.9510565162951535312, 1.000000000000000000, 0.9510565162951535312, 1.000000000000000000, 0.9510565162951535312, 1.000000000000000000, 0.9510565162951535312, 1.000000000000000000, 0.9510565162951535312, 1.000000000000000000, 0.9510565162951535312, 1.000000000000000000, 0.9510565162951535312, 1.000000000000000000, 0.9510565162951535312, 1.000000000000000000, 0.9510565162951535312, 1.000000000000000000, 0.9510565162951535312, 1.000000000000000000, 0.9510565162951535312, 1.000000000000000000, 0.9510565162951535312, 1.000000000000000000, 0.9510565162951535312, 1.000000000000000000, 0.9510565162951535312, 1.000000000000000000, 0.9510565162951535312, 1.000000000000000000, 0.9510565162951535312, 1.000000000000000000, 0.9510565162951535312, 1.000000000000000000, 0.9510565162951535312, 1.000000000000000000, 0.9510565162951535312, 1.000000000000000000, 0.9510565162951535312, 1.000000000000000000, 0.9510565162951535312, 1.000000000000000000, 0.9510565162951535312, 1.000000000000000000, 0.9510565162951535312, 1.000000000000000000),
 ( 0.3333333333333333703, 0.3170188387650512141, 0.3333333333333333703, 0.3170188387650512141, 0.3333333333333333703, 0.3170188387650512141, 0.3333333333333333703, 0.3170188387650512141, 0.3333333333333333703, 0.3170188387650512141, 0.3333333333333333703, 0.3170188387650512141, 0.3333333333333333703, 0.3170188387650512141, 0.3333333333333333703, 0.3170188387650512141, 0.3333333333333333703, 0.3170188387650512141, 0.3333333333333333703, 0.3170188387650512141, 0.3333333333333333703, 0.3170188387650512141, 0.3333333333333333703, 0.3170188387650512141, 0.3333333333333333703, 0.3170188387650512141, 0.3333333333333333703, 0.3170188387650512141, 0.3333333333333333703, 0.3170188387650512141, 0.3333333333333333703, 0.3170188387650512141, 0.3333333333333333703, 0.3170188387650512141, 0.3333333333333333703, 0.3170188387650512141, 0.3333333333333333703, 0.3170188387650512141, 0.3333333333333333703, 0.3170188387650512141, 0.3333333333333333703, 0.3170188387650512141, 0.3333333333333333703, 0.3170188387650512141, 0.3333333333333333703, 0.3170188387650512141, 0.3333333333333333703, 0.3170188387650512141, 0.3333333333333333703, 0.3170188387650512141, 0.3333333333333333703, 0.3170188387650512141, 0.3333333333333333703, 0.3170188387650512141, 0.3333333333333333703, 0.3170188387650512141, 0.3333333333333333703, 0.3170188387650512141, 0.3333333333333333703, 0.3170188387650512141, 0.3333333333333333703, 0.3170188387650512141, 0.3333333333333333703, 0.3170188387650512141, 0.3333333333333333703, 0.3170188387650512141, 0.3333333333333333703, 0.3170188387650512141, 0.3333333333333333703, 0.3170188387650512141, 0.3333333333333333703, 0.3170188387650512141, 0.3333333333333333703, 0.3170188387650512141, 0.3333333333333333703, 0.3170188387650512141, 0.3333333333333333703, 0.3170188387650512141, 0.3333333333333333703, 0.3170188387650512141, 0.3333333333333333703, 0.3170188387650512141, 0.3333333333333333703, 0.3170188387650512141, 0.3333333333333333703, 0.3170188387650512141, 0.3333333333333333703, 0.3170188387650512141, 0.3333333333333333703, 0.3170188387650512141, 0.3333333333333333703, 0.3170188387650512141, 0.3333333333333333703, 0.3170188387650512141, 0.3333333333333333703, 0.3170188387650512141, 0.3333333333333333703, 0.3170188387650512141, 0.3333333333333333703, 0.3170188387650512141, 0.3333333333333333703, 0.3170188387650512141, 0.3333333333333333703, 0.3170188387650512141, 0.3333333333333333703, 0.3170188387650512141, 0.3333333333333333703, 0.3170188387650512141, 0.3333333333333333703, 0.3170188387650512141, 0.3333333333333333703, 0.3170188387650512141, 0.3333333333333333703, 0.3170188387650512141, 0.3333333333333333703, 0.3170188387650512141, 0.3333333333333333703, 0.3170188387650512141, 0.3333333333333333703, 0.3170188387650512141, 0.3333333333333333703, 0.3170188387650512141, 0.3333333333333333703, 0.3170188387650512141, 0.3333333333333333703, 0.3170188387650512141, 0.3333333333333333703, 0.3170188387650512141, 0.3333333333333333703, 0.3170188387650512141, 0.3333333333333333703),
 ( 0.3333333333333333703, 0.3170188387650512141, 0.3333333333333333703, 0.3170188387650512141, 0.3333333333333333703, 0.3170188387650512141, 0.3333333333333333703, 0.3170188387650512141, 0.3333333333333333703, 0.3170188387650512141, 0.3333333333333333703, 0.3170188387650512141, 0.3333333333333333703, 0.3170188387650512141, 0.3333333333333333703, 0.3170188387650512141, 0.3333333333333333703, 0.3170188387650512141, 0.3333333333333333703, 0.3170188387650512141, 0.3333333333333333703, 0.3170188387650512141, 0.3333333333333333703, 0.3170188387650512141, 0.3333333333333333703, 0.3170188387650512141, 0.3333333333333333703, 0.3170188387650512141, 0.3333333333333333703, 0.3170188387650512141, 0.3333333333333333703, 0.3170188387650512141, 0.3333333333333333703, 0.3170188387650512141, 0.3333333333333333703, 0.3170188387650512141, 0.3333333333333333703, 0.3170188387650512141, 0.3333333333333333703, 0.3170188387650512141, 0.3333333333333333703, 0.3170188387650512141, 0.3333333333333333703, 0.3170188387650512141, 0.3333333333333333703, 0.3170188387650512141, 0.3333333333333333703, 0.3170188387650512141, 0.3333333333333333703, 0.3170188387650512141, 0.3333333333333333703, 0.3170188387650512141, 0.3333333333333333703, 0.3170188387650512141, 0.3333333333333333703, 0.3170188387650512141, 0.3333333333333333703, 0.3170188387650512141, 0.3333333333333333703, 0.3170188387650512141, 0.3333333333333333703, 0.3170188387650512141, 0.3333333333333333703, 0.3170188387650512141, 0.3333333333333333703, 0.3170188387650512141, 0.3333333333333333703, 0.3170188387650512141, 0.3333333333333333703, 0.3170188387650512141, 0.3333333333333333703, 0.3170188387650512141, 0.3333333333333333703, 0.3170188387650512141, 0.3333333333333333703, 0.3170188387650512141, 0.3333333333333333703, 0.3170188387650512141, 0.3333333333333333703, 0.3170188387650512141, 0.3333333333333333703, 0.3170188387650512141, 0.3333333333333333703, 0.3170188387650512141, 0.3333333333333333703, 0.3170188387650512141, 0.3333333333333333703, 0.3170188387650512141, 0.3333333333333333703, 0.3170188387650512141, 0.3333333333333333703, 0.3170188387650512141, 0.3333333333333333703, 0.3170188387650512141, 0.3333333333333333703, 0.3170188387650512141, 0.3333333333333333703, 0.3170188387650512141, 0.3333333333333333703, 0.3170188387650512141, 0.3333333333333333703, 0.3170188387650512141, 0.3333333333333333703, 0.3170188387650512141, 0.3333333333333333703, 0.3170188387650512141, 0.3333333333333333703, 0.3170188387650512141, 0.3333333333333333703, 0.3170188387650512141, 0.3333333333333333703, 0.3170188387650512141, 0.3333333333333333703, 0.3170188387650512141, 0.3333333333333333703, 0.3170188387650512141, 0.3333333333333333703, 0.3170188387650512141, 0.3333333333333333703, 0.3170188387650512141, 0.3333333333333333703, 0.3170188387650512141, 0.3333333333333333703, 0.3170188387650512141, 0.3333333333333333703, 0.3170188387650512141, 0.3333333333333333703, 0.3170188387650512141, 0.3333333333333333703, 0.3170188387650512141, 0.3333333333333333703),
 ( 1.000000000000000000, 0.9510565162951535312, 1.000000000000000000, 0.9510565162951535312, 1.000000000000000000, 0.9510565162951535312, 1.000000000000000000, 0.9510565162951535312, 1.000000000000000000, 0.9510565162951535312, 1.000000000000000000, 0.9510565162951535312, 1.000000000000000000, 0.9510565162951535312, 1.000000000000000000, 0.9510565162951535312, 1.000000000000000000, 0.9510565162951535312, 1.000000000000000000, 0.9510565162951535312, 1.000000000000000000, 0.9510565162951535312, 1.000000000000000000, 0.9510565162951535312, 1.000000000000000000, 0.9510565162951535312, 1.000000000000000000, 0.9510565162951535312, 1.000000000000000000, 0.9510565162951535312, 1.000000000000000000, 0.9510565162951535312, 1.000000000000000000, 0.9510565162951535312, 1.000000000000000000, 0.9510565162951535312, 1.000000000000000000, 0.9510565162951535312, 1.000000000000000000, 0.9510565162951535312, 1.000000000000000000, 0.9510565162951535312, 1.000000000000000000, 0.9510565162951535312, 1.000000000000000000, 0.9510565162951535312, 1.000000000000000000, 0.9510565162951535312, 1.000000000000000000, 0.9510565162951535312, 1.000000000000000000, 0.9510565162951535312, 1.000000000000000000, 0.9510565162951535312, 1.000000000000000000, 0.9510565162951535312, 1.000000000000000000, 0.9510565162951535312, 1.000000000000000000, 0.9510565162951535312, 1.000000000000000000, 0.9510565162951535312, 1.000000000000000000, 0.9510565162951535312, 1.000000000000000000, 0.9510565162951535312, 1.000000000000000000, 0.9510565162951535312, 1.000000000000000000, 0.9510565162951535312, 1.000000000000000000, 0.9510565162951535312, 1.000000000000000000, 0.9510565162951535312, 1.000000000000000000, 0.9510565162951535312, 1.000000000000000000, 0.9510565162951535312, 1.000000000000000000, 0.9510565162951535312, 1.000000000000000000, 0.9510565162951535312, 1.000000000000000000, 0.9510565162951535312, 1.000000000000000000, 0.9510565162951535312, 1.000000000000000000, 0.9510565162951535312, 1.000000000000000000, 0.9510565162951535312, 1.000000000000000000, 0.9510565162951535312, 1.000000000000000000, 0.9510565162951535312, 1.000000000000000000, 0.9510565162951535312, 1.000000000000000000, 0.9510565162951535312, 1.000000000000000000, 0.9510565162951535312, 1.000000000000000000, 0.9510565162951535312, 1.000000000000000000, 0.9510565162951535312, 1.000000000000000000, 0.9510565162951535312, 1.000000000000000000, 0.9510565162951535312, 1.000000000000000000, 0.9510565162951535312, 1.000000000000000000, 0.9510565162951535312, 1.000000000000000000, 0.9510565162951535312, 1.000000000000000000, 0.9510565162951535312, 1.000000000000000000, 0.9510565162951535312, 1.000000000000000000, 0.9510565162951535312, 1.000000000000000000, 0.9510565162951535312, 1.000000000000000000, 0.9510565162951535312, 1.000000000000000000, 0.9510565162951535312, 1.000000000000000000, 0.9510565162951535312, 1.000000000000000000, 0.9510565162951535312, 1.000000000000000000),
 ( 0.3333333333333333703, 0.3170188387650512141, 0.3333333333333333703, 0.3170188387650512141, 0.3333333333333333703, 0.3170188387650512141, 0.3333333333333333703, 0.3170188387650512141, 0.3333333333333333703, 0.3170188387650512141, 0.3333333333333333703, 0.3170188387650512141, 0.3333333333333333703, 0.3170188387650512141, 0.3333333333333333703, 0.3170188387650512141, 0.3333333333333333703, 0.3170188387650512141, 0.3333333333333333703, 0.3170188387650512141, 0.3333333333333333703, 0.3170188387650512141, 0.3333333333333333703, 0.3170188387650512141, 0.3333333333333333703, 0.3170188387650512141, 0.3333333333333333703, 0.3170188387650512141, 0.3333333333333333703, 0.3170188387650512141, 0.3333333333333333703, 0.3170188387650512141, 0.3333333333333333703, 0.3170188387650512141, 0.3333333333333333703, 0.3170188387650512141, 0.3333333333333333703, 0.3170188387650512141, 0.3333333333333333703, 0.3170188387650512141, 0.3333333333333333703, 0.3170188387650512141, 0.3333333333333333703, 0.3170188387650512141, 0.3333333333333333703, 0.3170188387650512141, 0.3333333333333333703, 0.3170188387650512141, 0.3333333333333333703, 0.3170188387650512141, 0.3333333333333333703, 0.3170188387650512141, 0.3333333333333333703, 0.3170188387650512141, 0.3333333333333333703, 0.3170188387650512141, 0.3333333333333333703, 0.3170188387650512141, 0.3333333333333333703, 0.3170188387650512141, 0.3333333333333333703, 0.3170188387650512141, 0.3333333333333333703, 0.3170188387650512141, 0.3333333333333333703, 0.3170188387650512141, 0.3333333333333333703, 0.3170188387650512141, 0.3333333333333333703, 0.3170188387650512141, 0.3333333333333333703, 0.3170188387650512141, 0.3333333333333333703, 0.3170188387650512141, 0.3333333333333333703, 0.3170188387650512141, 0.3333333333333333703, 0.3170188387650512141, 0.3333333333333333703, 0.3170188387650512141, 0.3333333333333333703, 0.3170188387650512141, 0.3333333333333333703, 0.3170188387650512141, 0.3333333333333333703, 0.3170188387650512141, 0.3333333333333333703, 0.3170188387650512141, 0.3333333333333333703, 0.3170188387650512141, 0.3333333333333333703, 0.3170188387650512141, 0.3333333333333333703, 0.3170188387650512141, 0.3333333333333333703, 0.3170188387650512141, 0.3333333333333333703, 0.3170188387650512141, 0.3333333333333333703, 0.3170188387650512141, 0.3333333333333333703, 0.3170188387650512141, 0.3333333333333333703, 0.3170188387650512141, 0.3333333333333333703, 0.3170188387650512141, 0.3333333333333333703, 0.3170188387650512141, 0.3333333333333333703, 0.3170188387650512141, 0.3333333333333333703, 0.3170188387650512141, 0.3333333333333333703, 0.3170188387650512141, 0.3333333333333333703, 0.3170188387650512141, 0.3333333333333333703, 0.3170188387650512141, 0.3333333333333333703, 0.3170188387650512141, 0.3333333333333333703, 0.3170188387650512141, 0.3333333333333333703, 0.3170188387650512141, 0.3333333333333333703, 0.3170188387650512141, 0.3333333333333333703, 0.3170188387650512141, 0.3333333333333333703, 0.3170188387650512141, 0.3333333333333333703),
 ( 0.3333333333333333703, 0.3170188387650512141, 0.3333333333333333703, 0.3170188387650512141, 0.3333333333333333703, 0.3170188387650512141, 0.3333333333333333703, 0.3170188387650512141, 0.3333333333333333703, 0.3170188387650512141, 0.3333333333333333703, 0.3170188387650512141, 0.3333333333333333703, 0.3170188387650512141, 0.3333333333333333703, 0.3170188387650512141, 0.3333333333333333703, 0.3170188387650512141, 0.3333333333333333703, 0.3170188387650512141, 0.3333333333333333703, 0.3170188387650512141, 0.3333333333333333703, 0.3170188387650512141, 0.3333333333333333703, 0.3170188387650512141, 0.3333333333333333703, 0.3170188387650512141, 0.3333333333333333703, 0.3170188387650512141, 0.3333333333333333703, 0.3170188387650512141, 0.3333333333333333703, 0.3170188387650512141, 0.3333333333333333703, 0.3170188387650512141, 0.3333333333333333703, 0.3170188387650512141, 0.3333333333333333703, 0.3170188387650512141, 0.3333333333333333703, 0.3170188387650512141, 0.3333333333333333703, 0.3170188387650512141, 0.3333333333333333703, 0.3170188387650512141, 0.3333333333333333703, 0.3170188387650512141, 0.3333333333333333703, 0.3170188387650512141, 0.3333333333333333703, 0.3170188387650512141, 0.3333333333333333703, 0.3170188387650512141, 0.3333333333333333703, 0.3170188387650512141, 0.3333333333333333703, 0.3170188387650512141, 0.3333333333333333703, 0.3170188387650512141, 0.3333333333333333703, 0.3170188387650512141, 0.3333333333333333703, 0.3170188387650512141, 0.3333333333333333703, 0.3170188387650512141, 0.3333333333333333703, 0.3170188387650512141, 0.3333333333333333703, 0.3170188387650512141, 0.3333333333333333703, 0.3170188387650512141, 0.3333333333333333703, 0.3170188387650512141, 0.3333333333333333703, 0.3170188387650512141, 0.3333333333333333703, 0.3170188387650512141, 0.3333333333333333703, 0.3170188387650512141, 0.3333333333333333703, 0.3170188387650512141, 0.3333333333333333703, 0.3170188387650512141, 0.3333333333333333703, 0.3170188387650512141, 0.3333333333333333703, 0.3170188387650512141, 0.3333333333333333703, 0.3170188387650512141, 0.3333333333333333703, 0.3170188387650512141, 0.3333333333333333703, 0.3170188387650512141, 0.3333333333333333703, 0.3170188387650512141, 0.3333333333333333703, 0.3170188387650512141, 0.3333333333333333703, 0.3170188387650512141, 0.3333333333333333703, 0.3170188387650512141, 0.3333333333333333703, 0.3170188387650512141, 0.3333333333333333703, 0.3170188387650512141, 0.3333333333333333703, 0.3170188387650512141, 0.3333333333333333703, 0.3170188387650512141, 0.3333333333333333703, 0.3170188387650512141, 0.3333333333333333703, 0.3170188387650512141, 0.3333333333333333703, 0.3170188387650512141, 0.3333333333333333703, 0.3170188387650512141, 0.3333333333333333703, 0.3170188387650512141, 0.3333333333333333703, 0.3170188387650512141, 0.3333333333333333703, 0.3170188387650512141, 0.3333333333333333703, 0.3170188387650512141, 0.3333333333333333703, 0.3170188387650512141, 0.3333333333333333703, 0.3170188387650512141, 0.3333333333333333703),
 ( 1.000000000000000000, 0.9510565162951535312, 1.000000000000000000, 0.9510565162951535312, 1.000000000000000000, 0.9510565162951535312, 1.000000000000000000, 0.9510565162951535312, 1.000000000000000000, 0.9510565162951535312, 1.000000000000000000, 0.9510565162951535312, 1.000000000000000000, 0.9510565162951535312, 1.000000000000000000, 0.9510565162951535312, 1.000000000000000000, 0.9510565162951535312, 1.000000000000000000, 0.9510565162951535312, 1.000000000000000000, 0.9510565162951535312, 1.000000000000000000, 0.9510565162951535312, 1.000000000000000000, 0.9510565162951535312, 1.000000000000000000, 0.9510565162951535312, 1.000000000000000000, 0.9510565162951535312, 1.000000000000000000, 0.9510565162951535312, 1.000000000000000000, 0.9510565162951535312, 1.000000000000000000, 0.9510565162951535312, 1.000000000000000000, 0.9510565162951535312, 1.000000000000000000, 0.9510565162951535312, 1.000000000000000000, 0.9510565162951535312, 1.000000000000000000, 0.9510565162951535312, 1.000000000000000000, 0.9510565162951535312, 1.000000000000000000, 0.9510565162951535312, 1.000000000000000000, 0.9510565162951535312, 1.000000000000000000, 0.9510565162951535312, 1.000000000000000000, 0.9510565162951535312, 1.000000000000000000, 0.9510565162951535312, 1.000000000000000000, 0.9510565162951535312, 1.000000000000000000, 0.9510565162951535312, 1.000000000000000000, 0.9510565162951535312, 1.000000000000000000, 0.9510565162951535312, 1.000000000000000000, 0.9510565162951535312, 1.000000000000000000, 0.9510565162951535312, 1.000000000000000000, 0.9510565162951535312, 1.000000000000000000, 0.9510565162951535312, 1.000000000000000000, 0.9510565162951535312, 1.000000000000000000, 0.9510565162951535312, 1.000000000000000000, 0.9510565162951535312, 1.000000000000000000, 0.9510565162951535312, 1.000000000000000000, 0.9510565162951535312, 1.000000000000000000, 0.9510565162951535312, 1.000000000000000000, 0.9510565162951535312, 1.000000000000000000, 0.9510565162951535312, 1.000000000000000000, 0.9510565162951535312, 1.000000000000000000, 0.9510565162951535312, 1.000000000000000000, 0.9510565162951535312, 1.000000000000000000, 0.9510565162951535312, 1.000000000000000000, 0.9510565162951535312, 1.000000000000000000, 0.9510565162951535312, 1.000000000000000000, 0.9510565162951535312, 1.000000000000000000, 0.9510565162951535312, 1.000000000000000000, 0.9510565162951535312, 1.000000000000000000, 0.9510565162951535312, 1.000000000000000000, 0.9510565162951535312, 1.000000000000000000, 0.9510565162951535312, 1.000000000000000000, 0.9510565162951535312, 1.000000000000000000, 0.9510565162951535312, 1.000000000000000000, 0.9510565162951535312, 1.000000000000000000, 0.9510565162951535312, 1.000000000000000000, 0.9510565162951535312, 1.000000000000000000, 0.9510565162951535312, 1.000000000000000000, 0.9510565162951535312, 1.000000000000000000, 0.9510565162951535312, 1.000000000000000000, 0.9510565162951535312, 1.000000000000000000) ) ) 
 REPRESENTATION_ITEM ( '' )  SURFACE ( )  );
#5268 = CARTESIAN_POINT ( 'NONE',  ( 5.056896391392317724, -9.814260835640970626, 2.648862081921448119 ) ) ;
#5269 = CARTESIAN_POINT ( 'NONE',  ( 13.25633410266679313, -4.503970704919842305, 4.567388001802134667 ) ) ;
#5270 = ADVANCED_FACE ( 'NONE', ( #6559 ), #119, .F. ) ;
#5271 = CARTESIAN_POINT ( 'NONE',  ( -9.355568503977838901, -4.766900247265280832, 8.399999999999963052 ) ) ;
#5272 = CARTESIAN_POINT ( 'NONE',  ( 8.731428362939190890, -13.89598863503036164, 27.21428571428572241 ) ) ;
#5273 = CARTESIAN_POINT ( 'NONE',  ( -163.6819620139764595, -1.015622990690433936, 12.96116402481652408 ) ) ;
#5274 = CARTESIAN_POINT ( 'NONE',  ( 1.441234910513245149, 13.92619789766829008, 14.85310228751642470 ) ) ;
#5275 = CARTESIAN_POINT ( 'NONE',  ( -1.595456901104623348, 10.37818827243067155, -0.6988620819214501623 ) ) ;
#5277 = CIRCLE ( 'NONE', #3969, 20.00000000000000000 ) ;
#5276 = CARTESIAN_POINT ( 'NONE',  ( 7.098671581784200768, 7.027753727702831021, 2.751137918078555789 ) ) ;
#5278 = AXIS2_PLACEMENT_3D ( 'NONE', #5584, #9533, #7243 ) ;
#5279 = CARTESIAN_POINT ( 'NONE',  ( -167.0804693905882914, -0.5605331060369084240, 12.98865281316615317 ) ) ;
#5280 = CARTESIAN_POINT ( 'NONE',  ( -1.567502665446231180, -13.91197093850540334, 39.85714285714286120 ) ) ;
#5281 = CARTESIAN_POINT ( 'NONE',  ( -10.24623928997352351, -10.06191849875416899, 2.504040569626438728 ) ) ;
#5282 = ORIENTED_EDGE ( 'NONE', *, *, #8294, .F. ) ;
#5283 = CIRCLE ( 'NONE', #3318, 13.00000000000000000 ) ;
#5284 = CARTESIAN_POINT ( 'NONE',  ( -15.88516839912898071, -1.917699372586004980, 7.138816573230711171 ) ) ;
#5285 = AXIS2_PLACEMENT_3D ( 'NONE', #7316, #4213, #239 ) ;
#5286 = EDGE_CURVE ( 'NONE', #3468, #6536, #5331, .T. ) ;
#5287 = CARTESIAN_POINT ( 'NONE',  ( -58.00000000000001421, 0.000000000000000000, 0.000000000000000000 ) ) ;
#5288 = CIRCLE ( 'NONE', #9770, 16.00000000000000000 ) ;
#5289 = CARTESIAN_POINT ( 'NONE',  ( 5.420364854932001819, 15.49051278174644430, 25.07142857142858361 ) ) ;
#5290 = CARTESIAN_POINT ( 'NONE',  ( -165.0000000000000284, -1.734723475976807094E-15, 13.00000000000000355 ) ) ;
#5291 = DIRECTION ( 'NONE',  ( 0.000000000000000000, -1.000000000000000000, 0.000000000000000000 ) ) ;
#5292 = CARTESIAN_POINT ( 'NONE',  ( -158.0000000000000284, -6.938893903907228378E-15, 0.000000000000000000 ) ) ;
#5293 = CARTESIAN_POINT ( 'NONE',  ( -9.865911304835474738, -1.562606840307925626, 2.550000000000035350 ) ) ;
#5294 = CARTESIAN_POINT ( 'NONE',  ( -7.027753727702738651, -7.098671581784262941, 18.24886208192143044 ) ) ;
#5295 = CARTESIAN_POINT ( 'NONE',  ( -160.0000000000000284, -20.00000000000000711, 2.449293598294706907E-15 ) ) ;
#5296 = CARTESIAN_POINT ( 'NONE',  ( 5.164528828830335705, -15.14410076328347543, 19.43261199819785645 ) ) ;
#5297 = CARTESIAN_POINT ( 'NONE',  ( 13.89598863503046111, -8.731428362939032795, 38.78571428571429180 ) ) ;
#5298 = STYLED_ITEM ( 'NONE', ( #4067 ), #183 ) ;
#5299 = DIRECTION ( 'NONE',  ( 5.938629746412708042E-18, -0.05705644952114252016, -0.9983709538884039114 ) ) ;
#5300 = CARTESIAN_POINT ( 'NONE',  ( -15.91362231745475597, -1.665163862720028254, 15.14689771248357708 ) ) ;
#5301 = CARTESIAN_POINT ( 'NONE',  ( -13.91197093850538380, -1.567502665446387278, 29.14285714285714235 ) ) ;
#5302 = CARTESIAN_POINT ( 'NONE',  ( 13.89598863503046111, -8.731428362939032795, 8.785714285714293581 ) ) ;
#5303 = CARTESIAN_POINT ( 'NONE',  ( 5.284464991282756152, -15.10213328493384743, 45.42857142857143060 ) ) ;
#5304 = EDGE_LOOP ( 'NONE', ( #7513, #2269, #8105, #3706 ) ) ;
#5305 = CARTESIAN_POINT ( 'NONE',  ( -5.012215536711506658, 9.837026868206027785, 12.14999999999996305 ) ) ;
#5306 = LINE ( 'NONE', #8717, #329 ) ;
#5307 = CARTESIAN_POINT ( 'NONE',  ( -13.54758718765249625, -8.512513224245459753, 46.71428571428571530 ) ) ;
#5308 =( NAMED_UNIT ( * ) SI_UNIT ( $, .STERADIAN. ) SOLID_ANGLE_UNIT ( ) );
#5309 = CARTESIAN_POINT ( 'NONE',  ( 4.619798703721856192, 13.59724543428036725, 9.067388001802141773 ) ) ;
#5310 = CARTESIAN_POINT ( 'NONE',  ( 10.90442828429183919, 1.727091770866679532, 19.04999999999997939 ) ) ;
#5311 = CARTESIAN_POINT ( 'NONE',  ( 10.13893307789800957, 12.50873118924980609, 47.39553751340654486 ) ) ;
#5312 = APPLICATION_PROTOCOL_DEFINITION ( 'draft international standard', 'automotive_design', 1998, #8904 ) ;
#5313 = CARTESIAN_POINT ( 'NONE',  ( -1.607813917173034124, 14.26974319298267346, 30.64285714285714946 ) ) ;
#5314 = ADVANCED_FACE ( 'NONE', ( #7302 ), #7146, .F. ) ;
#5315 = CARTESIAN_POINT ( 'NONE',  ( -11.92174236212692051, -7.340858601238089420, 26.71832628391215536 ) ) ;
#5316 = ORIENTED_EDGE ( 'NONE', *, *, #4719, .T. ) ;
#5317 = EDGE_CURVE ( 'NONE', #2524, #1613, #545, .T. ) ;
#5318 = CARTESIAN_POINT ( 'NONE',  ( 7.750357176954296712, -12.08964793087877787, 41.21024514465928235 ) ) ;
#5319 = VERTEX_POINT ( 'NONE', #8754 ) ;
#5320 = DIRECTION ( 'NONE',  ( 1.000000000000000000, 0.000000000000000000, 0.000000000000000000 ) ) ;
#5321 = CARTESIAN_POINT ( 'NONE',  ( -5.297344310588352201, -15.53355953199867301, 24.06738800180213644 ) ) ;
#5322 = CARTESIAN_POINT ( 'NONE',  ( 2.000000000000001776, 0.000000000000000000, 0.000000000000000000 ) ) ;
#5323 = PRODUCT_DEFINITION_SHAPE ( 'NONE', 'NONE',  #10233 ) ;
#5324 = CARTESIAN_POINT ( 'NONE',  ( 8.442910196168311288, 4.355403765523574222, 1.898862081921442790 ) ) ;
#5325 = CARTESIAN_POINT ( 'NONE',  ( 9.809645194533960222, 9.989344678689363377, 51.49595943037355994 ) ) ;
#5326 = CARTESIAN_POINT ( 'NONE',  ( -7.806708723663830618, -7.806708723663901672, 5.250000000000008882 ) ) ;
#5327 = CARTESIAN_POINT ( 'NONE',  ( -7.424621202458789426, 7.424621202458724589, 0.000000000000000000 ) ) ;
#5328 = LINE ( 'NONE', #1408, #5131 ) ;
#5329 = CARTESIAN_POINT ( 'NONE',  ( 12.08964793087886314, -7.750357176954162597, 24.78975485534072476 ) ) ;
#5330 = PRESENTATION_STYLE_ASSIGNMENT (( #1101 ) ) ;
#5331 = CIRCLE ( 'NONE', #6974, 2.000000000000000000 ) ;
#5332 = CARTESIAN_POINT ( 'NONE',  ( 5.297344310588354865, 15.53355953199867301, 51.06738800180214355 ) ) ;
#5333 = CARTESIAN_POINT ( 'NONE',  ( 9.355568503977840678, 4.766900247265305701, 0.9000000000000119016 ) ) ;
#5334 = DIRECTION ( 'NONE',  ( 1.000000000000000000, 0.000000000000000000, 0.000000000000000000 ) ) ;
#5335 = AXIS2_PLACEMENT_3D ( 'NONE', #8705, #7094, #2200 ) ;
#5336 = CARTESIAN_POINT ( 'NONE',  ( 4.743843029824831525, -13.17239914596749095, 11.42453085894499587 ) ) ;
#5337 = CARTESIAN_POINT ( 'NONE',  ( 1.612135949262739398, 9.858066664633913234, 11.45113791807854220 ) ) ;
#5338 = CARTESIAN_POINT ( 'NONE',  ( -8.486213763410637156, -4.270415729527911708, 1.401137918078568134 ) ) ;
#5339 = DIRECTION ( 'NONE',  ( 1.000000000000000000, 4.755747939841215952E-17, -0.000000000000000000 ) ) ;
#5340 = CARTESIAN_POINT ( 'NONE',  ( -11.22385875690717327, 11.40355824106234550, 46.00404056962644006 ) ) ;
#5341 = CARTESIAN_POINT ( 'NONE',  ( -4.623906867372410190, 13.21436662431711895, 42.42857142857143060 ) ) ;
#5342 = ADVANCED_FACE ( 'NONE', ( #7248 ), #169, .T. ) ;
#5343 = CARTESIAN_POINT ( 'NONE',  ( 11.92174236212692229, 7.340858601238088532, -0.2816737160878517443 ) ) ;
#5344 = ORIENTED_EDGE ( 'NONE', *, *, #6195, .T. ) ;
#5345 = CARTESIAN_POINT ( 'NONE',  ( -13.96533075980324234, 8.621071003556515677, 7.781673716087849968 ) ) ;
#5346 = CARTESIAN_POINT ( 'NONE',  ( -1.925929944387235853E-31, -1.018491042385001544, -1.270000000000007123 ) ) ;
#5347 = CARTESIAN_POINT ( 'NONE',  ( 15.10213328493390783, -5.284464991282587398, 26.57142857142857295 ) ) ;
#5348 = FACE_OUTER_BOUND ( 'NONE', #8939, .T. ) ;
#5349 = DIRECTION ( 'NONE',  ( -1.000000000000000000, -1.387778780781445676E-16, -0.000000000000000000 ) ) ;
#5350 = DIRECTION ( 'NONE',  ( 1.000000000000000000, 0.000000000000000000, 0.000000000000000000 ) ) ;
#5351 = CARTESIAN_POINT ( 'NONE',  ( -8.900167166472156666, 4.534861676072234893, 11.84999999999997478 ) ) ;
#5352 = CARTESIAN_POINT ( 'NONE',  ( -1.533232399700100057, 9.375578539472089190, 13.29886208192143471 ) ) ;
#5353 = CARTESIAN_POINT ( 'NONE',  ( -7.071067811865514585, 7.071067811865452413, 0.000000000000000000 ) ) ;
#5354 = CARTESIAN_POINT ( 'NONE',  ( 10.03895970123120307, 12.58845729673829972, 49.39149694378009769 ) ) ;
#5355 = CARTESIAN_POINT ( 'NONE',  ( 16.29368510291089223, -1.967016585148476882, 24.36118342676929416 ) ) ;
#5356 = CARTESIAN_POINT ( 'NONE',  ( -5.284464991282755264, 15.10213328493384743, 18.42857142857143415 ) ) ;
#5357 = CARTESIAN_POINT ( 'NONE',  ( 0.1896486214910092227, 16.00782165069140817, 48.73000000000003951 ) ) ;
#5358 = ORIENTED_EDGE ( 'NONE', *, *, #8807, .F. ) ;
#5359 = CARTESIAN_POINT ( 'NONE',  ( -9.355568503977838901, -4.766900247265280832, 14.39999999999996838 ) ) ;
#5360 = ORIENTED_EDGE ( 'NONE', *, *, #7171, .F. ) ;
#5361 = CARTESIAN_POINT ( 'NONE',  ( 1.791431617652837316, 15.89939535829188877, 42.85714285714285410 ) ) ;
#5362 = CARTESIAN_POINT ( 'NONE',  ( 10.89658364409024749, 1.776620879821585897, 11.04886208192144359 ) ) ;
#5363 = CARTESIAN_POINT ( 'NONE',  ( 13.54758718765249803, 8.512513224245457977, 1.714285714285716855 ) ) ;
#5364 = CARTESIAN_POINT ( 'NONE',  ( -13.54758718765249625, -8.512513224245459753, 4.714285714285712636 ) ) ;
#5365 = CARTESIAN_POINT ( 'NONE',  ( 12.15899005565164792, -7.639999817571654361, 26.78571428571429180 ) ) ;
#5366 = CARTESIAN_POINT ( 'NONE',  ( -1.693770420379220099, -13.89774397934251837, 37.86118342676929416 ) ) ;
#5367 = CARTESIAN_POINT ( 'NONE',  ( 8.464561979789474222, 4.312909747525755400, 9.900000000000019895 ) ) ;
#5368 = CARTESIAN_POINT ( 'NONE',  ( -12.22833218042443271, 7.529642458189139909, 37.78167371608785174 ) ) ;
#5369 = ORIENTED_EDGE ( 'NONE', *, *, #9792, .T. ) ;
#5370 = FACE_BOUND ( 'NONE', #5472, .T. ) ;
#5371 = CARTESIAN_POINT ( 'NONE',  ( -11.40355824106246807, 11.22385875690704715, 19.99595943037356349 ) ) ;
#5372 = CARTESIAN_POINT ( 'NONE',  ( -1.837501619626327853, 16.30827793483733856, 6.642857142857143238 ) ) ;
#5373 = CARTESIAN_POINT ( 'NONE',  ( 1.513077731352925115, 9.873755945037103743, 10.44886208192141908 ) ) ;
#5374 = CARTESIAN_POINT ( 'NONE',  ( 13.96533075980324234, -8.621071003556521006, 28.78167371608785174 ) ) ;
#5375 = DIRECTION ( 'NONE',  ( -0.7071067811865510144, 0.7071067811865440200, -6.116266257073745883E-17 ) ) ;
#5376 = CARTESIAN_POINT ( 'NONE',  ( -9.814260835641038128, 5.056896391392219137, 10.85113791807856209 ) ) ;
#5377 = CARTESIAN_POINT ( 'NONE',  ( 0.2000000000000057288, 0.000000000000000000, 0.000000000000000000 ) ) ;
#5378 = CARTESIAN_POINT ( 'NONE',  ( 8.884063115244108744, 10.93517402715751885, 47.39553751340654486 ) ) ;
#5379 =( LENGTH_UNIT ( ) NAMED_UNIT ( * ) SI_UNIT ( .MILLI., .METRE. ) );
#5380 = CARTESIAN_POINT ( 'NONE',  ( 13.51115193377584589, 4.865839792409294873, 3.924530858944990541 ) ) ;
#5381 = CARTESIAN_POINT ( 'NONE',  ( 5.012215536711512875, -9.837026868206002916, 4.650000000000027001 ) ) ;
#5382 = CARTESIAN_POINT ( 'NONE',  ( -4.619798703721853528, -13.59724543428036725, 30.06738800180214355 ) ) ;
#5383 = CARTESIAN_POINT ( 'NONE',  ( -7.098671581784199880, -7.027753727702804376, 16.25113791807856245 ) ) ;
#5384 = CARTESIAN_POINT ( 'NONE',  ( 4.490180821391514421, -8.922933199037132113, 0.6511379180785785703 ) ) ;
#5385 = DIRECTION ( 'NONE',  ( -1.000000000000000000, -1.387778780781445676E-16, -0.000000000000000000 ) ) ;
#5386 = CARTESIAN_POINT ( 'NONE',  ( -4.742819248065502258, -13.55419868402813677, 40.07142857142857650 ) ) ;
#5387 = CARTESIAN_POINT ( 'NONE',  ( -13.59724543428031573, -4.619798703722008959, 2.932611998197868886 ) ) ;
#5388 = ORIENTED_EDGE ( 'NONE', *, *, #7171, .T. ) ;
#5389 = CARTESIAN_POINT ( 'NONE',  ( 15.14410076328353227, -5.164528828830166063, 10.56738800180213644 ) ) ;
#5391 = CARTESIAN_POINT ( 'NONE',  ( 0.000000000000000000, -0.8865213383406761460, 1.535499999999911935 ) ) ;
#5390 = AXIS2_PLACEMENT_3D ( 'NONE', #117, #7198, #1820 ) ;
#5392 = CARTESIAN_POINT ( 'NONE',  ( -11.31370849898482156, 11.31370849898469544, 30.00000000000000355 ) ) ;
#5393 = CARTESIAN_POINT ( 'NONE',  ( 2.000000000000001776, 1.773042676681366281, 0.000000000000000000 ) ) ;
#5394 = FACE_BOUND ( 'NONE', #1255, .T. ) ;
#5395 = APPLICATION_CONTEXT ( 'automotive_design' ) ;
#5396 = CARTESIAN_POINT ( 'NONE',  ( 4.534861676072320158, -8.900167166472096270, 7.649999999999992362 ) ) ;
#5397 = CARTESIAN_POINT ( 'NONE',  ( -8.442910196168309511, -4.355403765523546689, 18.39886208192140771 ) ) ;
#5398 = FACE_OUTER_BOUND ( 'NONE', #7953, .T. ) ;
#5399 = CARTESIAN_POINT ( 'NONE',  ( -1.917699372585823570, -15.88516839912900558, 19.86118342676929416 ) ) ;
#5400 = CARTESIAN_POINT ( 'NONE',  ( 16.30827793483735633, -1.837501619626142890, 38.35714285714287541 ) ) ;
#5401 = CARTESIAN_POINT ( 'NONE',  ( -15.53355953199861794, -5.297344310588530725, 14.93261199819787066 ) ) ;
#5402 = EDGE_CURVE ( 'NONE', #913, #594, #6412, .T. ) ;
#5403 = CARTESIAN_POINT ( 'NONE',  ( 13.54758718765249803, 8.512513224245457977, 19.71428571428571175 ) ) ;
#5404 = LINE ( 'NONE', #1435, #9092 ) ;
#5405 = CARTESIAN_POINT ( 'NONE',  ( 9.837026868206066865, -5.012215536711395636, 16.35000000000000497 ) ) ;
#5406 = ORIENTED_EDGE ( 'NONE', *, *, #2720, .F. ) ;
#5407 = CARTESIAN_POINT ( 'NONE',  ( -11.31370849898482156, 11.31370849898469544, 42.00000000000000000 ) ) ;
#5408 =( GEOMETRIC_REPRESENTATION_CONTEXT ( 3 ) GLOBAL_UNCERTAINTY_ASSIGNED_CONTEXT ( ( #9905 ) ) GLOBAL_UNIT_ASSIGNED_CONTEXT ( ( #5427, #5482, #7858 ) ) REPRESENTATION_CONTEXT ( 'NONE', 'WORKASPACE' ) );
#5409 = CARTESIAN_POINT ( 'NONE',  ( -5.056896391392315948, 9.814260835640997271, 10.14886208192142725 ) ) ;
#5410 = CARTESIAN_POINT ( 'NONE',  ( 8.512513224245308763, 13.54758718765259040, 7.285714285714284699 ) ) ;
#5411 = CARTESIAN_POINT ( 'NONE',  ( -15.06016580658428694, 5.404401153735006957, 45.57546914105501656 ) ) ;
#5412 = CARTESIAN_POINT ( 'NONE',  ( 10.15407889436379030, 10.15407889436390221, 19.50000000000000355 ) ) ;
#5413 = CARTESIAN_POINT ( 'NONE',  ( 13.92619789766827587, 1.441234910513398582, 36.14689771248357886 ) ) ;
#5414 = CARTESIAN_POINT ( 'NONE',  ( -4.534861676072319270, 8.900167166472122915, 12.14999999999996483 ) ) ;
#5415 = ORIENTED_EDGE ( 'NONE', *, *, #9157, .T. ) ;
#5416 = CARTESIAN_POINT ( 'NONE',  ( -1.737328882695368115, 14.25515036105620581, 38.63881657323070584 ) ) ;
#5417 = PRODUCT_DEFINITION_FORMATION_WITH_SPECIFIED_SOURCE ( 'ANY', '', #3525, .NOT_KNOWN. ) ;
#5418 = ORIENTED_EDGE ( 'NONE', *, *, #2060, .T. ) ;
#5419 = DIRECTION ( 'NONE',  ( 0.000000000000000000, 8.191099868251446680E-34, 1.000000000000000000 ) ) ;
#5420 = CARTESIAN_POINT ( 'NONE',  ( 16.32287076676382043, -1.707986654103810897, 22.35310228751642114 ) ) ;
#5421 = CARTESIAN_POINT ( 'NONE',  ( 16.30827793483735633, -1.837501619626142890, 8.357142857142855874 ) ) ;
#5422 = CARTESIAN_POINT ( 'NONE',  ( 4.579542530753127672, -8.877401133907065756, 11.64886208192146988 ) ) ;
#5423 = CARTESIAN_POINT ( 'NONE',  ( -1.665163862719845067, -15.91362231745477374, 17.85310228751642114 ) ) ;
#5424 = CARTESIAN_POINT ( 'NONE',  ( -10.90442828429183919, -1.727091770866654663, 2.550000000000035350 ) ) ;
#5425 = CARTESIAN_POINT ( 'NONE',  ( -7.842167650704559456, -7.771249796623176387, 16.25113791807856245 ) ) ;
#5426 = CARTESIAN_POINT ( 'NONE',  ( 2.000000000000001776, -0.8865213383406761460, 1.535499999999911935 ) ) ;
#5427 =( LENGTH_UNIT ( ) NAMED_UNIT ( * ) SI_UNIT ( .MILLI., .METRE. ) );
#5428 = CARTESIAN_POINT ( 'NONE',  ( -4.743843029824828861, 13.17239914596749450, 8.424530858944992318 ) ) ;
#5429 = CARTESIAN_POINT ( 'NONE',  ( 7.424621202458790314, -7.424621202458697944, 7.500000000000007105 ) ) ;
#5430 = CARTESIAN_POINT ( 'NONE',  ( 16.30827793483735633, -1.837501619626142890, 32.35714285714286120 ) ) ;
#5431 = DIRECTION ( 'NONE',  ( 1.000000000000000000, 0.000000000000000000, 0.000000000000000000 ) ) ;
#5432 = CARTESIAN_POINT ( 'NONE',  ( 13.89774397934249706, 1.693770420379375308, 28.13881657323070939 ) ) ;
#5433 = CARTESIAN_POINT ( 'NONE',  ( 7.390897758835871301, -7.458344646081617846, 9.501137918078587319 ) ) ;
#5434 = CARTESIAN_POINT ( 'NONE',  ( 9.375578539472099848, -1.533232399699987702, 0.2011379180785754783 ) ) ;
#5435 = CARTESIAN_POINT ( 'NONE',  ( -166.8775874622578783, -1.084229144011057411, 12.95729691005224637 ) ) ;
#5436 = CARTESIAN_POINT ( 'NONE',  ( 11.40355824106234550, 11.22385875690717327, 47.50404056962644006 ) ) ;
#5437 = CARTESIAN_POINT ( 'NONE',  ( 1.693770420379222319, 13.89774397934251837, 10.86118342676929238 ) ) ;
#5438 = CARTESIAN_POINT ( 'NONE',  ( 13.92619789766827587, 1.441234910513398582, 0.1468977124835755543 ) ) ;
#5439 = ORIENTED_EDGE ( 'NONE', *, *, #4659, .F. ) ;
#5440 = EDGE_CURVE ( 'NONE', #10061, #6680, #4201, .T. ) ;
#5441 = CARTESIAN_POINT ( 'NONE',  ( 16.32287076676382043, -1.707986654103810897, 4.353102287516421143 ) ) ;
#5442 = DIRECTION ( 'NONE',  ( -4.755747939841216568E-17, 1.000000000000000000, 0.000000000000000000 ) ) ;
#5443 = EDGE_CURVE ( 'NONE', #4112, #1810, #2682, .T. ) ;
#5444 = CARTESIAN_POINT ( 'NONE',  ( 15.49051278174638036, 5.420364854932175014, 37.92857142857143060 ) ) ;
#5445 = CARTESIAN_POINT ( 'NONE',  ( -70.00000000000001421, 8.500000000000000000, 0.000000000000000000 ) ) ;
#5446 = LINE ( 'NONE', #8607, #3960 ) ;
#5447 = CARTESIAN_POINT ( 'NONE',  ( 8.900167166472154889, -4.534861676072210912, 13.34999999999998188 ) ) ;
#5448 = CARTESIAN_POINT ( 'NONE',  ( 9.390499931835536884, -1.439022436064273158, 20.19886208192146526 ) ) ;
#5449 = CARTESIAN_POINT ( 'NONE',  ( -70.00000000000001421, 1.959434878635765131E-15, -16.00000000000000000 ) ) ;
#5450 = CARTESIAN_POINT ( 'NONE',  ( -9.865911304835474738, -1.562606840307925626, 2.550000000000035794 ) ) ;
#5451 = CARTESIAN_POINT ( 'NONE',  ( 8.621071003556677326, -13.96533075980314287, 19.21832628391215181 ) ) ;
#5452 = CIRCLE ( 'NONE', #7102, 20.00000000000000000 ) ;
#5453 = CIRCLE ( 'NONE', #7434, 13.00000000000000000 ) ;
#5454 = AXIS2_PLACEMENT_3D ( 'NONE', #9021, #1112, #1930 ) ;
#5455 = CARTESIAN_POINT ( 'NONE',  ( -8.512513224245306986, -13.54758718765259218, 16.28571428571428470 ) ) ;
#5456 = DIRECTION ( 'NONE',  ( 1.000000000000000000, 4.755747939841215952E-17, -0.000000000000000000 ) ) ;
#5457 = CARTESIAN_POINT ( 'NONE',  ( -15.49051278174638036, -5.420364854932175902, 4.928571428571430602 ) ) ;
#5458 =( NAMED_UNIT ( * ) SI_UNIT ( $, .STERADIAN. ) SOLID_ANGLE_UNIT ( ) );
#5459 = CARTESIAN_POINT ( 'NONE',  ( 13.89598863503045933, -8.731428362939032795, 44.78571428571429180 ) ) ;
#5460 = CIRCLE ( 'NONE', #2504, 16.99999999999997868 ) ;
#5461 = COLOUR_RGB ( '', 0.66274510, 0.83137255, 0.94901961) ;
#5462 = CIRCLE ( 'NONE', #3981, 0.2000000000000000944 ) ;
#5463 = CARTESIAN_POINT ( 'NONE',  ( 9.333916720356675967, 4.809394265263123636, 4.898862081921403266 ) ) ;
#5464 = CARTESIAN_POINT ( 'NONE',  ( -16.30827793483735988, 1.837501619626141780, 5.357142857142856762 ) ) ;
#5465 = CARTESIAN_POINT ( 'NONE',  ( 15.10213328493390783, -5.284464991282587398, 2.571428571428571619 ) ) ;
#5466 = CARTESIAN_POINT ( 'NONE',  ( 13.21436662431716869, -4.623906867372263640, 38.57142857142857650 ) ) ;
#5467 = EDGE_CURVE ( 'NONE', #928, #4112, #224, .T. ) ;
#5468 = CARTESIAN_POINT ( 'NONE',  ( -4.865839792409144771, -13.51115193377589740, 32.07546914105502367 ) ) ;
#5469 = CARTESIAN_POINT ( 'NONE',  ( -6.717514421272238856, 6.717514421272181124, 12.00000000000001066 ) ) ;
#5470 =( GEOMETRIC_REPRESENTATION_CONTEXT ( 3 ) GLOBAL_UNCERTAINTY_ASSIGNED_CONTEXT ( ( #5147 ) ) GLOBAL_UNIT_ASSIGNED_CONTEXT ( ( #113, #1770, #1054 ) ) REPRESENTATION_CONTEXT ( 'NONE', 'WORKASPACE' ) );
#5471 = CARTESIAN_POINT ( 'NONE',  ( 9.837026868206066865, -5.012215536711392083, 13.34999999999998188 ) ) ;
#5472 = EDGE_LOOP ( 'NONE', ( #2308, #6066 ) ) ;
#5473 = CARTESIAN_POINT ( 'NONE',  ( 1.737328882695370558, -14.25515036105620581, 35.63881657323071295 ) ) ;
#5474 = DIRECTION ( 'NONE',  ( 0.000000000000000000, 0.000000000000000000, 1.000000000000000000 ) ) ;
#5475 = CARTESIAN_POINT ( 'NONE',  ( -15.14410076328353227, 5.164528828830164287, 25.56738800180213644 ) ) ;
#5476 = CARTESIAN_POINT ( 'NONE',  ( 11.31370849898482334, -11.31370849898469366, 9.000000000000001776 ) ) ;
#5477 = CARTESIAN_POINT ( 'NONE',  ( 5.297344310588354865, 15.53355953199867301, 21.06738800180213644 ) ) ;
#5478 = CARTESIAN_POINT ( 'NONE',  ( -1.642561882922479732, 10.37072757624895303, 0.2999999999999669598 ) ) ;
#5480 = CLOSED_SHELL ( 'NONE', ( #8027, #211, #1175, #1476, #561, #2885, #5154, #7882, #932 ) ) ;
#5479 = CARTESIAN_POINT ( 'NONE',  ( -9.355568503977838901, -4.766900247265280832, 2.400000000000013234 ) ) ;
#5481 = DIRECTION ( 'NONE',  ( 0.000000000000000000, -6.338944243255235518E-49, 1.000000000000000000 ) ) ;
#5482 =( NAMED_UNIT ( * ) PLANE_ANGLE_UNIT ( ) SI_UNIT ( $, .RADIAN. ) );
#5483 = CARTESIAN_POINT ( 'NONE',  ( 13.89598863503046111, -8.731428362939032795, 32.78571428571430602 ) ) ;
#5484 = ORIENTED_EDGE ( 'NONE', *, *, #5776, .F. ) ;
#5485 = EDGE_CURVE ( 'NONE', #1692, #4209, #3018, .T. ) ;
#5486 = CARTESIAN_POINT ( 'NONE',  ( 14.28433602490915000, -1.478298951650544479, 4.353102287516421143 ) ) ;
#5487 = CARTESIAN_POINT ( 'NONE',  ( -1.642561882922479732, 10.37072757624895303, 0.2999999999999669598 ) ) ;
#5488 = CARTESIAN_POINT ( 'NONE',  ( -5.284464991282755264, 15.10213328493384743, 12.42857142857142705 ) ) ;
#5489 = FACE_OUTER_BOUND ( 'NONE', #3256, .T. ) ;
#5490 = CARTESIAN_POINT ( 'NONE',  ( -7.390897758835869524, 7.458344646081644491, 5.001137918078545574 ) ) ;
#5491 = CARTESIAN_POINT ( 'NONE',  ( 9.873755945037075321, 1.513077731353044131, 18.05113791807859513 ) ) ;
#5492 = CARTESIAN_POINT ( 'NONE',  ( -163.2909762424711460, -1.312104824217039889, 12.93415009021162554 ) ) ;
#5493 = CARTESIAN_POINT ( 'NONE',  ( 13.17239914596754424, -4.743843029824685864, 6.575469141055007682 ) ) ;
#5494 = VECTOR ( 'NONE', #1454, 1000.000000000000000 ) ;
#5495 = CARTESIAN_POINT ( 'NONE',  ( -12.08964793087886314, 7.750357176954159932, 15.78975485534072121 ) ) ;
#5496 = CARTESIAN_POINT ( 'NONE',  ( 15.44746603149413922, 5.543385399275817527, 9.924530858944988765 ) ) ;
#5497 = CARTESIAN_POINT ( 'NONE',  ( -55.00000000000002132, 1.249000902703378022E-16, 18.00000000000001776 ) ) ;
#5498 = CARTESIAN_POINT ( 'NONE',  ( 15.49051278174638036, 5.420364854932175014, 43.92857142857143060 ) ) ;
#5499 = PLANE ( 'NONE',  #4842 ) ;
#5500 = DIRECTION ( 'NONE',  ( -6.162975822039153635E-32, -0.5000000000000011102, -0.8660254037844379305 ) ) ;
#5501 = CARTESIAN_POINT ( 'NONE',  ( 4.312909747525650594, 8.464561979789532842, 15.60000000000000320 ) ) ;
#5502 = CARTESIAN_POINT ( 'NONE',  ( -1.533232399700100057, 9.375578539472098072, 16.29886208192143471 ) ) ;
#5503 = DIRECTION ( 'NONE',  ( 0.000000000000000000, 8.191099868251446680E-34, 1.000000000000000000 ) ) ;
#5504 = EDGE_CURVE ( 'NONE', #3063, #6295, #8470, .T. ) ;
#5505 = CARTESIAN_POINT ( 'NONE',  ( -1.707986654103994528, 16.32287076676380266, 22.64689771248357530 ) ) ;
#5506 = CARTESIAN_POINT ( 'NONE',  ( -6.717514421272238856, 6.717514421272176683, 3.000000000000002665 ) ) ;
#5507 = CARTESIAN_POINT ( 'NONE',  ( -13.61519076058348254, -8.404922754268771001, 38.71832628391214826 ) ) ;
#5508 = CARTESIAN_POINT ( 'NONE',  ( -15.89939535829186923, -1.791431617653016062, 17.14285714285713880 ) ) ;
#5509 = DIRECTION ( 'NONE',  ( -1.000000000000000000, 4.575525868300071581E-16, 0.000000000000000000 ) ) ;
#5510 = CARTESIAN_POINT ( 'NONE',  ( 15.89939535829187278, 1.791431617653015174, 8.142857142857145902 ) ) ;
#5511 =( NAMED_UNIT ( * ) PLANE_ANGLE_UNIT ( ) SI_UNIT ( $, .RADIAN. ) );
#5512 = FILL_AREA_STYLE_COLOUR ( '', #5461 ) ;
#5513 = AXIS2_PLACEMENT_3D ( 'NONE', #7491, #468, #314 ) ;
#5514 = CARTESIAN_POINT ( 'NONE',  ( 1.677562661911645714, 10.91227292449346464, 4.448862081921434175 ) ) ;
#5515 = CARTESIAN_POINT ( 'NONE',  ( -4.865839792409144771, -13.51115193377589740, 44.07546914105503078 ) ) ;
#5516 = CARTESIAN_POINT ( 'NONE',  ( -13.54758718765249625, -8.512513224245459753, 10.71428571428571708 ) ) ;
#5517 = CARTESIAN_POINT ( 'NONE',  ( -14.26974319298268767, 1.607813917172874696, 35.35714285714286120 ) ) ;
#5518 = CARTESIAN_POINT ( 'NONE',  ( -14.25515036105622890, 1.737328882695209575, 39.36118342676930837 ) ) ;
#5519 = CARTESIAN_POINT ( 'NONE',  ( -1.562606840307830591, -9.865911304835481843, 13.95000000000002416 ) ) ;
#5520 = CARTESIAN_POINT ( 'NONE',  ( -9.355568503977838901, -4.766900247265280832, 14.39999999999996838 ) ) ;
#5521 = ORIENTED_EDGE ( 'NONE', *, *, #5747, .T. ) ;
#5522 = CARTESIAN_POINT ( 'NONE',  ( 4.619798703721856192, 13.59724543428036725, 51.06738800180214355 ) ) ;
#5523 = ORIENTED_EDGE ( 'NONE', *, *, #417, .T. ) ;
#5524 = CARTESIAN_POINT ( 'NONE',  ( -11.51250119794888072, -11.69682198916848037, 30.49595943037356349 ) ) ;
#5525 = CARTESIAN_POINT ( 'NONE',  ( -15.89939535829186923, -1.791431617653016062, 17.14285714285713880 ) ) ;
#5526 = CARTESIAN_POINT ( 'NONE',  ( 15.14410076328353227, -5.164528828830166063, 22.56738800180214000 ) ) ;
#5527 = CARTESIAN_POINT ( 'NONE',  ( 10.90442828429183919, 1.727091770866679532, 1.049999999999966738 ) ) ;
#5528 = CARTESIAN_POINT ( 'NONE',  ( -10.90442828429183919, -1.727091770866655329, 8.549999999999963407 ) ) ;
#5529 = FACE_OUTER_BOUND ( 'NONE', #3169, .T. ) ;
#5530 = CARTESIAN_POINT ( 'NONE',  ( 11.31370849898482334, -11.31370849898469366, 33.00000000000000000 ) ) ;
#5531 = EDGE_LOOP ( 'NONE', ( #8199, #8633 ) ) ;
#5532 = CARTESIAN_POINT ( 'NONE',  ( -1.441234910513241818, -13.92619789766829008, 17.85310228751642114 ) ) ;
#5533 = APPLICATION_CONTEXT ( 'automotive_design' ) ;
#5534 = CARTESIAN_POINT ( 'NONE',  ( 10.90442828429184274, 1.727091770866679310, 10.05000000000003268 ) ) ;
#5535 = FACE_BOUND ( 'NONE', #3876, .T. ) ;
#5536 = CARTESIAN_POINT ( 'NONE',  ( -13.25633410266679313, 4.503970704919840529, 25.56738800180213644 ) ) ;
#5537 = CARTESIAN_POINT ( 'NONE',  ( -7.842167650704559456, -7.771249796623180828, 4.251137918078595312 ) ) ;
#5538 = CARTESIAN_POINT ( 'NONE',  ( -4.355403765523468529, -8.442910196168352144, 13.10113791807856920 ) ) ;
#5539 = LINE ( 'NONE', #8857, #3634 ) ;
#5540 = CARTESIAN_POINT ( 'NONE',  ( -12.08964793087886314, 7.750357176954159932, 3.789754855340718542 ) ) ;
#5541 = CARTESIAN_POINT ( 'NONE',  ( -4.503970704919988854, 13.25633410266674517, 16.43261199819786356 ) ) ;
#5542 = ORIENTED_EDGE ( 'NONE', *, *, #1274, .T. ) ;
#5543 = CARTESIAN_POINT ( 'NONE',  ( 11.40355824106246985, -11.22385875690704538, 16.99595943037355994 ) ) ;
#5544 = DIRECTION ( 'NONE',  ( 1.000000000000000000, 0.000000000000000000, 0.000000000000000000 ) ) ;
#5545 = CARTESIAN_POINT ( 'NONE',  ( 1.791431617652837316, 15.89939535829188877, 48.85714285714286120 ) ) ;
#5546 = FACE_OUTER_BOUND ( 'NONE', #3502, .T. ) ;
#5547 = CARTESIAN_POINT ( 'NONE',  ( -2.000000000000002665, 16.99999999999997868, 0.000000000000000000 ) ) ;
#5548 = CARTESIAN_POINT ( 'NONE',  ( -1.486127417882243895, 9.383039235653816590, 15.29999999999997939 ) ) ;
#5549 = CARTESIAN_POINT ( 'NONE',  ( 8.900167166472154889, -4.534861676072210024, 4.350000000000036948 ) ) ;
#5550 = CARTESIAN_POINT ( 'NONE',  ( -164.3074826167014351, 2.040297258018446858, 12.83900971347711639 ) ) ;
#5551 = CARTESIAN_POINT ( 'NONE',  ( -15.53355953199861794, -5.297344310588530725, 26.93261199819786356 ) ) ;
#5552 = CARTESIAN_POINT ( 'NONE',  ( 1.486127417882244783, -9.383039235653791721, 1.800000000000023803 ) ) ;
#5553 = CARTESIAN_POINT ( 'NONE',  ( -1.917699372585823570, -15.88516839912900558, 37.86118342676929416 ) ) ;
#5554 = ORIENTED_EDGE ( 'NONE', *, *, #1185, .T. ) ;
#5555 = CARTESIAN_POINT ( 'NONE',  ( 15.89939535829187278, 1.791431617653015174, 14.14285714285714413 ) ) ;
#5556 = CARTESIAN_POINT ( 'NONE',  ( -158.0000000000000284, 17.99999999999999645, 2.204364238465235822E-15 ) ) ;
#5557 = CARTESIAN_POINT ( 'NONE',  ( -11.31370849898482156, 11.31370849898469544, 5.999999999999998224 ) ) ;
#5558 = FILL_AREA_STYLE ('',( #7112 ) ) ;
#5559 = CARTESIAN_POINT ( 'NONE',  ( 6.751237864895159646, -6.683790977649239906, 2.498862081921459755 ) ) ;
#5560 = CARTESIAN_POINT ( 'NONE',  ( 7.458344646081711105, -7.390897758835778930, 5.498862081921462419 ) ) ;
#5561 = CARTESIAN_POINT ( 'NONE',  ( 1.707986654103998303, -16.32287076676380266, 1.646897712483578857 ) ) ;
#5562 = CARTESIAN_POINT ( 'NONE',  ( 5.284464991282756152, -15.10213328493384743, 9.428571428571425272 ) ) ;
#5563 = CARTESIAN_POINT ( 'NONE',  ( -10.15407889436378852, -10.15407889436390398, 40.50000000000000000 ) ) ;
#5564 = CARTESIAN_POINT ( 'NONE',  ( 14.25515036105622535, -1.737328882695210241, 36.36118342676930126 ) ) ;
#5565 = EDGE_CURVE ( 'NONE', #5950, #6730, #1261, .T. ) ;
#5566 = CARTESIAN_POINT ( 'NONE',  ( 13.92619789766827587, 1.441234910513398582, 30.14689771248358241 ) ) ;
#5567 = CARTESIAN_POINT ( 'NONE',  ( -9.865911304835474738, -1.562606840307925848, 5.549999999999998934 ) ) ;
#5568 = CARTESIAN_POINT ( 'NONE',  ( 9.355568503977840678, 4.766900247265305701, 18.90000000000002700 ) ) ;
#5569 = CARTESIAN_POINT ( 'NONE',  ( -1.607813917173034124, 14.26974319298267524, 0.6428571428571432378 ) ) ;
#5570 = CARTESIAN_POINT ( 'NONE',  ( 7.133621909761823559E-16, -15.00000000000000000, 1.836970198721029589E-15 ) ) ;
#5571 = CARTESIAN_POINT ( 'NONE',  ( -1.837501619626327853, 16.30827793483733856, 18.64285714285715301 ) ) ;
#5572 = CARTESIAN_POINT ( 'NONE',  ( -15.14410076328353227, 5.164528828830164287, 25.56738800180213644 ) ) ;
#5573 = CARTESIAN_POINT ( 'NONE',  ( 4.766900247265192903, 9.355568503977902850, 3.599999999999992095 ) ) ;
#5574 = CARTESIAN_POINT ( 'NONE',  ( -10.90442828429183919, -1.727091770866654663, 2.550000000000035350 ) ) ;
#5575 = CARTESIAN_POINT ( 'NONE',  ( -7.639999817571786700, 12.15899005565156266, 0.2142857142857168273 ) ) ;
#5576 = AXIS2_PLACEMENT_3D ( 'NONE', #4333, #4548, #6684 ) ;
#5577 = ORIENTED_EDGE ( 'NONE', *, *, #3196, .F. ) ;
#5578 = CARTESIAN_POINT ( 'NONE',  ( 4.619798703721856192, 13.59724543428036725, 15.06738800180213822 ) ) ;
#5579 = CARTESIAN_POINT ( 'NONE',  ( -4.766900247265192014, -9.355568503977876205, 14.10000000000000142 ) ) ;
#5580 = CARTESIAN_POINT ( 'NONE',  ( 5.284464991282756152, -15.10213328493384743, 9.428571428571425272 ) ) ;
#5581 = CARTESIAN_POINT ( 'NONE',  ( -166.0062384261120769, 1.312070622931204689, 12.93375722677777340 ) ) ;
#5582 = CARTESIAN_POINT ( 'NONE',  ( -9.814260835641038128, 5.056896391392219137, 1.851137918078540334 ) ) ;
#5583 = CARTESIAN_POINT ( 'NONE',  ( -7.098671581784199880, -7.027753727702804376, 16.25113791807856245 ) ) ;
#5584 = CARTESIAN_POINT ( 'NONE',  ( 57.99999999999997158, 0.000000000000000000, 0.000000000000000000 ) ) ;
#5585 = CARTESIAN_POINT ( 'NONE',  ( 12.08964793087886314, -7.750357176954162597, 12.78975485534072121 ) ) ;
#5586 = SHAPE_REPRESENTATION ( 'base support', ( #3995 ), #3161 ) ;
#5587 = EDGE_CURVE ( 'NONE', #7530, #5864, #3515, .T. ) ;
#5588 = CARTESIAN_POINT ( 'NONE',  ( 10.24623928997352884, 10.06191849875416899, 11.50404056962644006 ) ) ;
#5589 = ORIENTED_EDGE ( 'NONE', *, *, #4371, .T. ) ;
#5590 = DIRECTION ( 'NONE',  ( -1.000000000000000000, 0.000000000000000000, 0.000000000000000000 ) ) ;
#5591 = CARTESIAN_POINT ( 'NONE',  ( -13.89598863503046111, 8.731428362939027465, 41.78571428571430602 ) ) ;
#5592 = CARTESIAN_POINT ( 'NONE',  ( -164.8920828308066859, -1.650077165904365373, 12.89485344440482173 ) ) ;
#5593 = FACE_BOUND ( 'NONE', #103, .T. ) ;
#5594 = CARTESIAN_POINT ( 'NONE',  ( -9.865911304835474738, -1.562606840307925626, 17.55000000000002913 ) ) ;
#5595 = CARTESIAN_POINT ( 'NONE',  ( 4.312909747525650594, 8.464561979789541724, 6.599999999999994316 ) ) ;
#5596 = CARTESIAN_POINT ( 'NONE',  ( -163.6886816470472468, 1.709539868520255412, 12.88734415733343752 ) ) ;
#5597 = CARTESIAN_POINT ( 'NONE',  ( 13.61519076058348254, 8.404922754268771001, 23.71832628391215181 ) ) ;
#5598 = CARTESIAN_POINT ( 'NONE',  ( 6.717514421272239744, -6.717514421272154479, 4.500000000000003553 ) ) ;
#5599 = CARTESIAN_POINT ( 'NONE',  ( -8.621071003556675549, 13.96533075980314642, 40.21832628391215536 ) ) ;
#5600 = EDGE_CURVE ( 'NONE', #4587, #3374, #9304, .T. ) ;
#5601 = ORIENTED_EDGE ( 'NONE', *, *, #7907, .T. ) ;
#5602 = CARTESIAN_POINT ( 'NONE',  ( -1.837501619626328297, 16.30827793483733856, 24.64285714285714235 ) ) ;
#5603 = CARTESIAN_POINT ( 'NONE',  ( 3.890496870457673229, 14.43432932945637504, -1.604941620322696453E-32 ) ) ;
#5604 = PRODUCT_DEFINITION ( 'UNKNOWN', '', #7888, #7116 ) ;
#5605 = CARTESIAN_POINT ( 'NONE',  ( 15.10213328493390783, -5.284464991282587398, 8.571428571428569398 ) ) ;
#5606 = DIRECTION ( 'NONE',  ( 0.000000000000000000, 0.000000000000000000, 1.000000000000000000 ) ) ;
#5607 = CARTESIAN_POINT ( 'NONE',  ( 1.533232399700100945, -9.375578539472067874, 8.798862081921429379 ) ) ;
#5608 = CARTESIAN_POINT ( 'NONE',  ( 10.37818827243067510, -1.595456901104499225, 20.19886208192146526 ) ) ;
#5609 = CARTESIAN_POINT ( 'NONE',  ( -1.677562661911643938, -10.91227292449344688, 14.94886208192145105 ) ) ;
#5610 = CARTESIAN_POINT ( 'NONE',  ( -8.620103694221995738, -13.47998361472161299, 2.289754855340722539 ) ) ;
#5611 = AXIS2_PLACEMENT_3D ( 'NONE', #1628, #3017, #9338 ) ;
#5612 = CARTESIAN_POINT ( 'NONE',  ( 15.10213328493390783, -5.284464991282587398, 20.57142857142857295 ) ) ;
#5613 = CIRCLE ( 'NONE', #9922, 1.816100000000000270 ) ;
#5614 = CARTESIAN_POINT ( 'NONE',  ( -1.607813917173034124, 14.26974319298267346, 36.64285714285714590 ) ) ;
#5615 = CARTESIAN_POINT ( 'NONE',  ( 1.478298951650704351, -14.28433602490913579, 37.64689771248358596 ) ) ;
#5616 = CARTESIAN_POINT ( 'NONE',  ( 13.91197093850538380, 1.567502665446386390, 8.142857142857145902 ) ) ;
#5617 = DIRECTION ( 'NONE',  ( -1.000000000000000000, 4.575525868300071581E-16, 0.000000000000000000 ) ) ;
#5618 = CARTESIAN_POINT ( 'NONE',  ( -5.056896391392315948, 9.814260835640997271, 1.148862081921408151 ) ) ;
#5619 = ORIENTED_EDGE ( 'NONE', *, *, #8383, .F. ) ;
#5620 = CARTESIAN_POINT ( 'NONE',  ( -7.639999817571787588, 12.15899005565156266, 6.214285714285717965 ) ) ;
#5621 = CIRCLE ( 'NONE', #4800, 8.000000000000000000 ) ;
#5622 = ORIENTED_EDGE ( 'NONE', *, *, #1997, .T. ) ;
#5623 = CARTESIAN_POINT ( 'NONE',  ( -8.787954181158717404, -8.913453481710840620, -1.270000000000007123 ) ) ;
#5624 = VECTOR ( 'NONE', #5833, 1000.000000000000000 ) ;
#5625 = CARTESIAN_POINT ( 'NONE',  ( 15.89939535829187278, 1.791431617653015174, 20.14285714285714235 ) ) ;
#5626 = CARTESIAN_POINT ( 'NONE',  ( -11.40355824106246807, 11.22385875690704715, 43.99595943037355994 ) ) ;
#5627 = CARTESIAN_POINT ( 'NONE',  ( 1.642561882922480621, -10.37072757624891750, 10.80000000000003268 ) ) ;
#5628 = CARTESIAN_POINT ( 'NONE',  ( 9.837026868206066865, -5.012215536711391195, 4.350000000000036948 ) ) ;
#5629 = DIRECTION ( 'NONE',  ( 1.000000000000000000, 1.387778780781445676E-16, 0.000000000000000000 ) ) ;
#5630 = ADVANCED_FACE ( 'NONE', ( #3619 ), #3531, .T. ) ;
#5631 = VECTOR ( 'NONE', #4774, 1000.000000000000114 ) ;
#5632 = VERTEX_POINT ( 'NONE', #3681 ) ;
#5633 = CARTESIAN_POINT ( 'NONE',  ( -12.22833218042443271, 7.529642458189139909, 19.78167371608784819 ) ) ;
#5634 = CARTESIAN_POINT ( 'NONE',  ( 10.37072757624895836, -1.642561882922356498, 16.19999999999999218 ) ) ;
#5635 = CARTESIAN_POINT ( 'NONE',  ( -8.512513224245306986, -13.54758718765259218, 16.28571428571428470 ) ) ;
#5636 = CARTESIAN_POINT ( 'NONE',  ( -163.6878309682295765, 1.006148260057784238, 12.96131713918894235 ) ) ;
#5637 = CARTESIAN_POINT ( 'NONE',  ( -1.737328882695368115, 14.25515036105620581, 44.63881657323071295 ) ) ;
#5638 = CARTESIAN_POINT ( 'NONE',  ( -1.776620879821455556, -10.89658364409025637, 6.951137918078597266 ) ) ;
#5639 = CARTESIAN_POINT ( 'NONE',  ( -1.439022436064386845, 9.390499931835526226, 11.30113791807855961 ) ) ;
#5640 = LINE ( 'NONE', #7193, #8427 ) ;
#5641 = CARTESIAN_POINT ( 'NONE',  ( 13.92619789766827587, 1.441234910513398582, 0.1468977124835755543 ) ) ;
#5642 = SURFACE_STYLE_FILL_AREA ( #2491 ) ;
#5643 = CARTESIAN_POINT ( 'NONE',  ( 1.693770420379222319, 13.89774397934251837, 10.86118342676929238 ) ) ;
#5644 = ORIENTED_EDGE ( 'NONE', *, *, #9435, .F. ) ;
#5645 = DIRECTION ( 'NONE',  ( 1.000000000000000000, 4.755747939841215952E-17, -0.000000000000000000 ) ) ;
#5646 = CARTESIAN_POINT ( 'NONE',  ( -11.40355824106246807, 11.22385875690704715, 1.995959430373561272 ) ) ;
#5647 = DIRECTION ( 'NONE',  ( 1.000000000000000000, 0.000000000000000000, 0.000000000000000000 ) ) ;
#5648 = DIRECTION ( 'NONE',  ( 1.000000000000000000, 0.000000000000000000, 0.000000000000000000 ) ) ;
#5649 = CARTESIAN_POINT ( 'NONE',  ( 6.717514421272239744, -6.717514421272154479, 19.50000000000001776 ) ) ;
#5650 = CARTESIAN_POINT ( 'NONE',  ( 9.865911304835474738, 1.562606840307949829, 7.050000000000010481 ) ) ;
#5651 = DIRECTION ( 'NONE',  ( 0.000000000000000000, 0.000000000000000000, 1.000000000000000000 ) ) ;
#5652 = CARTESIAN_POINT ( 'NONE',  ( -8.620103694221995738, -13.47998361472161299, 26.28975485534072831 ) ) ;
#5653 = CARTESIAN_POINT ( 'NONE',  ( -1.486127417882243895, 9.383039235653816590, 0.2999999999999669598 ) ) ;
#5654 = CARTESIAN_POINT ( 'NONE',  ( 13.61519076058348254, 8.404922754268771001, 35.71832628391214115 ) ) ;
#5655 = VERTEX_POINT ( 'NONE', #7454 ) ;
#5656 = ADVANCED_FACE ( 'NONE', ( #4513, #5074, #9942 ), #2896, .F. ) ;
#5657 = CARTESIAN_POINT ( 'NONE',  ( 5.284464991282756152, -15.10213328493384743, 27.42857142857143060 ) ) ;
#5658 = CARTESIAN_POINT ( 'NONE',  ( 3.773891550226160518, 14.38788920816386785, -1.793508096673563358E-16 ) ) ;
#5659 = VECTOR ( 'NONE', #9066, 1000.000000000000000 ) ;
#5660 = CARTESIAN_POINT ( 'NONE',  ( 1.791431617652837316, 15.89939535829188877, 0.8571428571428549859 ) ) ;
#5661 = SURFACE_STYLE_FILL_AREA ( #2512 ) ;
#5662 = CARTESIAN_POINT ( 'NONE',  ( -8.922933199037192509, 4.490180821391428267, 9.848862081921437195 ) ) ;
#5663 = CARTESIAN_POINT ( 'NONE',  ( 1.677562661911645714, 10.91227292449347175, 19.44886208192144039 ) ) ;
#5664 = CARTESIAN_POINT ( 'NONE',  ( 9.809645194534072132, -9.989344678689256796, 43.00404056962644717 ) ) ;
#5665 = CARTESIAN_POINT ( 'NONE',  ( 13.54758718765249803, 8.512513224245457977, 13.71428571428571352 ) ) ;
#5666 = CARTESIAN_POINT ( 'NONE',  ( 14.26974319298268767, -1.607813917172876472, 38.35714285714286831 ) ) ;
#5667 = CARTESIAN_POINT ( 'NONE',  ( 1.917699372585825790, 15.88516839912900203, -1.138816573230706286 ) ) ;
#5668 = CARTESIAN_POINT ( 'NONE',  ( 11.85413878919593422, 7.448449071214774619, 13.71428571428571352 ) ) ;
#5669 = CARTESIAN_POINT ( 'NONE',  ( -1.562606840307830591, -9.865911304835481843, 16.94999999999998863 ) ) ;
#5670 = CARTESIAN_POINT ( 'NONE',  ( 10.37818827243067510, -1.595456901104500780, 8.198862081921454603 ) ) ;
#5671 = EDGE_LOOP ( 'NONE', ( #7619, #3211, #2718, #5801 ) ) ;
#5672 = CARTESIAN_POINT ( 'NONE',  ( 1.567502665446232957, 13.91197093850540156, 0.8571428571428549859 ) ) ;
#5673 = ORIENTED_EDGE ( 'NONE', *, *, #1055, .F. ) ;
#5674 = DIRECTION ( 'NONE',  ( 0.000000000000000000, -8.191099868251446680E-34, -1.000000000000000000 ) ) ;
#5675 = CIRCLE ( 'NONE', #3369, 8.200000000000009948 ) ;
#5676 = CARTESIAN_POINT ( 'NONE',  ( -8.731428362939187338, 13.89598863503036164, 24.21428571428571530 ) ) ;
#5677 = CARTESIAN_POINT ( 'NONE',  ( 5.297344310588354865, 15.53355953199867301, 39.06738800180213644 ) ) ;
#5678 = CARTESIAN_POINT ( 'NONE',  ( 9.837026868206066865, -5.012215536711392083, 7.350000000000000533 ) ) ;
#5679 = CARTESIAN_POINT ( 'NONE',  ( -9.837026868206066865, 5.012215536711413399, 2.849999999999968114 ) ) ;
#5680 = CARTESIAN_POINT ( 'NONE',  ( 14.26974319298268767, -1.607813917172876472, 2.357142857142856762 ) ) ;
#5681 = ORIENTED_EDGE ( 'NONE', *, *, #2684, .T. ) ;
#5682 = CARTESIAN_POINT ( 'NONE',  ( -9.837026868206070418, 5.012215536711412511, 8.850000000000010303 ) ) ;
#5683 = CARTESIAN_POINT ( 'NONE',  ( -68.00000000000001421, 1.040949779275250140E-15, -8.500000000000000000 ) ) ;
#5684 = CARTESIAN_POINT ( 'NONE',  ( -1.441234910513241818, -13.92619789766829008, 35.85310228751641404 ) ) ;
#5685 = CARTESIAN_POINT ( 'NONE',  ( -10.91227292449344155, -1.677562661911749187, 13.55113791807856316 ) ) ;
#5686 = CARTESIAN_POINT ( 'NONE',  ( 8.486213763410640709, 4.270415729527941018, 11.90113791807857702 ) ) ;
#5687 = DIRECTION ( 'NONE',  ( 1.000000000000000000, 0.000000000000000000, 0.000000000000000000 ) ) ;
#5688 = CARTESIAN_POINT ( 'NONE',  ( 10.24623928997352884, 10.06191849875416899, 17.50404056962643651 ) ) ;
#5689 =( LENGTH_UNIT ( ) NAMED_UNIT ( * ) SI_UNIT ( .MILLI., .METRE. ) );
#5690 = CARTESIAN_POINT ( 'NONE',  ( 1.478298951650704351, -14.28433602490913579, 13.64689771248357708 ) ) ;
#5691 = ORIENTED_EDGE ( 'NONE', *, *, #1300, .F. ) ;
#5692 = CARTESIAN_POINT ( 'NONE',  ( -5.986002070941136566, -13.58603705635637482, -1.270000000000007123 ) ) ;
#5693 = CARTESIAN_POINT ( 'NONE',  ( 5.297344310588354865, 15.53355953199867301, 15.06738800180213822 ) ) ;
#5694 = CARTESIAN_POINT ( 'NONE',  ( -88.00000000000002842, 9.797174393178825657E-16, -8.000000000000000000 ) ) ;
#5695 = DIRECTION ( 'NONE',  ( 0.000000000000000000, 6.938893903907221444E-18, 1.000000000000000000 ) ) ;
#5696 = CARTESIAN_POINT ( 'NONE',  ( -4.490180821391513533, 8.922933199037158758, 8.151137918078559252 ) ) ;
#5697 = CARTESIAN_POINT ( 'NONE',  ( -7.063212654743466601, -7.063212654743531438, 5.250000000000008882 ) ) ;
#5698 = DIRECTION ( 'NONE',  ( 1.000000000000000000, 0.000000000000000000, 0.000000000000000000 ) ) ;
#5699 = CARTESIAN_POINT ( 'NONE',  ( 1.707986654103998303, -16.32287076676380266, 25.64689771248357886 ) ) ;
#5700 = CARTESIAN_POINT ( 'NONE',  ( 4.742819248065503146, 13.55419868402813677, 31.07142857142857295 ) ) ;
#5701 = CARTESIAN_POINT ( 'NONE',  ( 15.53355953199861794, 5.297344310588528060, 35.93261199819787066 ) ) ;
#5702 = ORIENTED_EDGE ( 'NONE', *, *, #6775, .F. ) ;
#5703 = CARTESIAN_POINT ( 'NONE',  ( -15.49051278174638036, -5.420364854932175902, 28.92857142857143771 ) ) ;
#5704 = DIRECTION ( 'NONE',  ( -0.000000000000000000, -0.000000000000000000, 1.000000000000000000 ) ) ;
#5705 = CARTESIAN_POINT ( 'NONE',  ( -16.30827793483735988, 1.837501619626141780, 17.35714285714286476 ) ) ;
#5706 =( NAMED_UNIT ( * ) SI_UNIT ( $, .STERADIAN. ) SOLID_ANGLE_UNIT ( ) );
#5707 = CARTESIAN_POINT ( 'NONE',  ( -7.458344646081709328, 7.390897758835805575, 18.99886208192142334 ) ) ;
#5708 = CARTESIAN_POINT ( 'NONE',  ( 7.556039541191335474, 11.78653521626503320, 47.28975485534072476 ) ) ;
#5709 = CARTESIAN_POINT ( 'NONE',  ( -13.89598863503046111, 8.731428362939027465, 17.78571428571428115 ) ) ;
#5710 = FILL_AREA_STYLE_COLOUR ( '', #3327 ) ;
#5711 = CARTESIAN_POINT ( 'NONE',  ( -13.17239914596754424, 4.743843029824683200, 39.57546914105500946 ) ) ;
#5712 = CARTESIAN_POINT ( 'NONE',  ( 4.623906867372411078, -13.21436662431711717, 9.428571428571425272 ) ) ;
#5713 = EDGE_CURVE ( 'NONE', #3104, #9748, #7610, .T. ) ;
#5714 = DIRECTION ( 'NONE',  ( 0.8571673007021101132, 0.000000000000000000, 0.5150380749100580413 ) ) ;
#5715 = CARTESIAN_POINT ( 'NONE',  ( -10.37818827243067688, 1.595456901104523428, 12.69886208192145816 ) ) ;
#5716 = VERTEX_POINT ( 'NONE', #6754 ) ;
#5717 = CARTESIAN_POINT ( 'NONE',  ( -9.899494936611716867, 9.899494936611610285, 11.99999999999999645 ) ) ;
#5718 = VERTEX_POINT ( 'NONE', #7669 ) ;
#5719 = CARTESIAN_POINT ( 'NONE',  ( 4.200000000000009059, 0.000000000000000000, 0.000000000000000000 ) ) ;
#5720 = CIRCLE ( 'NONE', #6867, 0.9906000000000003691 ) ;
#5721 = CARTESIAN_POINT ( 'NONE',  ( -15.10213328493390961, 5.284464991282586510, 17.57142857142856940 ) ) ;
#5722 = CARTESIAN_POINT ( 'NONE',  ( 15.88516839912898071, 1.917699372586004092, 40.13881657323070584 ) ) ;
#5723 =( REPRESENTATION_RELATIONSHIP ('NONE','NONE', #58, #8907 ) REPRESENTATION_RELATIONSHIP_WITH_TRANSFORMATION ( #3133 )SHAPE_REPRESENTATION_RELATIONSHIP( ) );
#5724 = CARTESIAN_POINT ( 'NONE',  ( 4.766900247265192903, 9.355568503977911732, 6.599999999999994316 ) ) ;
#5725 = CARTESIAN_POINT ( 'NONE',  ( -1.642561882922479732, 10.37072757624895303, 18.29999999999998295 ) ) ;
#5726 = CARTESIAN_POINT ( 'NONE',  ( 9.899494936611718643, -9.899494936611608509, 15.00000000000000000 ) ) ;
#5727 = AXIS2_PLACEMENT_3D ( 'NONE', #1452, #4702, #3664 ) ;
#5728 = ORIENTED_EDGE ( 'NONE', *, *, #1473, .T. ) ;
#5729 = CARTESIAN_POINT ( 'NONE',  ( -14.28433602490915000, 1.478298951650542481, 13.35310228751641937 ) ) ;
#5730 = CARTESIAN_POINT ( 'NONE',  ( -1.727091770866549414, -10.90442828429184807, 16.94999999999998863 ) ) ;
#5731 = DIRECTION ( 'NONE',  ( 0.000000000000000000, 8.191099868251446680E-34, 1.000000000000000000 ) ) ;
#5732 = CARTESIAN_POINT ( 'NONE',  ( 13.51115193377584589, 4.865839792409294873, 33.92453085894499054 ) ) ;
#5733 = CARTESIAN_POINT ( 'NONE',  ( 1.776620879821457333, 10.89658364409027236, 14.45113791807853509 ) ) ;
#5734 = CARTESIAN_POINT ( 'NONE',  ( 4.809394265263009061, 9.333916720356739916, 8.601137918078563871 ) ) ;
#5735 = MECHANICAL_DESIGN_GEOMETRIC_PRESENTATION_REPRESENTATION (  '', ( #7384 ), #5408 ) ;
#5736 = DIRECTION ( 'NONE',  ( 1.000000000000000000, 4.755747939841215952E-17, -0.000000000000000000 ) ) ;
#5737 = PLANE ( 'NONE',  #7538 ) ;
#5738 = CARTESIAN_POINT ( 'NONE',  ( -15.14410076328353227, 5.164528828830164287, 7.567388001802139108 ) ) ;
#5739 = CARTESIAN_POINT ( 'NONE',  ( -13.47998361472151174, -8.620103694222146729, 24.71024514465928235 ) ) ;
#5740 = DIRECTION ( 'NONE',  ( -1.000000000000000000, -0.000000000000000000, -0.000000000000000000 ) ) ;
#5741 = CARTESIAN_POINT ( 'NONE',  ( -162.8500000000000227, -0.2807562947469993686, 14.99999999999999822 ) ) ;
#5742 = CARTESIAN_POINT ( 'NONE',  ( 8.486213763410640709, 4.270415729527937465, 8.901137918078571687 ) ) ;
#5743 = CARTESIAN_POINT ( 'NONE',  ( 8.464561979789474222, 4.312909747525755400, 3.899999999999959055 ) ) ;
#5744 = CARTESIAN_POINT ( 'NONE',  ( -163.5798452441948427, 1.620402670652003829, 12.89900989023366407 ) ) ;
#5745 = CARTESIAN_POINT ( 'NONE',  ( 1.607813917173038121, -14.26974319298267346, 33.64285714285715301 ) ) ;
#5746 = CARTESIAN_POINT ( 'NONE',  ( 13.82664651025767100, -8.841785722321541030, 42.78975485534072476 ) ) ;
#5747 = EDGE_CURVE ( 'NONE', #3031, #4901, #4404, .T. ) ;
#5748 = EDGE_CURVE ( 'NONE', #1613, #2524, #1205, .T. ) ;
#5749 = ORIENTED_EDGE ( 'NONE', *, *, #7762, .F. ) ;
#5750 = CARTESIAN_POINT ( 'NONE',  ( -1.837501619626328297, 16.30827793483733856, 30.64285714285715301 ) ) ;
#5751 = CARTESIAN_POINT ( 'NONE',  ( 2.266096533192709206, 14.38188575653963319, -1.488941479308426028E-16 ) ) ;
#5752 = CARTESIAN_POINT ( 'NONE',  ( -1.837501619626328297, 16.30827793483733856, 12.64285714285714235 ) ) ;
#5753 =( NAMED_UNIT ( * ) PLANE_ANGLE_UNIT ( ) SI_UNIT ( $, .RADIAN. ) );
#5754 = CARTESIAN_POINT ( 'NONE',  ( -9.858066664633883036, -1.612135949262831547, 18.54886208192142405 ) ) ;
#5755 = CARTESIAN_POINT ( 'NONE',  ( 4.724406229267374968, 9.377220287599060455, 19.59886208192140700 ) ) ;
#5756 = UNCERTAINTY_MEASURE_WITH_UNIT (LENGTH_MEASURE( 1.000000000000000082E-05 ), #7886, 'distance_accuracy_value', 'NONE');
#5757 = CARTESIAN_POINT ( 'NONE',  ( -11.69682198916834892, -11.51250119794901394, 14.50404056962643651 ) ) ;
#5758 = CARTESIAN_POINT ( 'NONE',  ( -5.420364854931999155, -15.49051278174644253, 34.07142857142859071 ) ) ;
#5759 = CARTESIAN_POINT ( 'NONE',  ( 2.000000000000001776, 0.000000000000000000, 0.000000000000000000 ) ) ;
#5760 = CARTESIAN_POINT ( 'NONE',  ( 15.06016580658428694, -5.404401153735007846, 0.5754691410550027975 ) ) ;
#5761 = CARTESIAN_POINT ( 'NONE',  ( 9.899494936611718643, -9.899494936611608509, 15.00000000000000000 ) ) ;
#5762 = CARTESIAN_POINT ( 'NONE',  ( -4.312909747525649706, -8.464561979789507973, 17.10000000000000497 ) ) ;
#5763 = CARTESIAN_POINT ( 'NONE',  ( 1.677562661911645714, 10.91227292449347175, 7.448862081921427070 ) ) ;
#5764 = ORIENTED_EDGE ( 'NONE', *, *, #4544, .F. ) ;
#5765 = CARTESIAN_POINT ( 'NONE',  ( -13.91197093850538380, -1.567502665446387278, 23.14285714285714590 ) ) ;
#5766 = ORIENTED_EDGE ( 'NONE', *, *, #7551, .F. ) ;
#5767 = CARTESIAN_POINT ( 'NONE',  ( -8.512513224245306986, -13.54758718765259218, 28.28571428571428825 ) ) ;
#5768 = CIRCLE ( 'NONE', #9421, 18.00000000000000355 ) ;
#5769 = CARTESIAN_POINT ( 'NONE',  ( -16.32287076676382398, 1.707986654103809343, 31.35310228751642470 ) ) ;
#5770 = CARTESIAN_POINT ( 'NONE',  ( -1.642561882922479732, 10.37072757624896191, 6.299999999999972289 ) ) ;
#5771 = CARTESIAN_POINT ( 'NONE',  ( 10.90442828429183919, 1.727091770866679532, 19.04999999999997939 ) ) ;
#5772 = EDGE_CURVE ( 'NONE', #6421, #10061, #7971, .T. ) ;
#5773 = CARTESIAN_POINT ( 'NONE',  ( -14.26974319298268767, 1.607813917172874696, 11.35714285714285765 ) ) ;
#5774 = CIRCLE ( 'NONE', #4640, 16.99999999999997868 ) ;
#5775 = VECTOR ( 'NONE', #2702, 1000.000000000000000 ) ;
#5776 = EDGE_CURVE ( 'NONE', #9748, #1651, #8973, .T. ) ;
#5777 = CARTESIAN_POINT ( 'NONE',  ( 1.441234910513245149, 13.92619789766829008, 32.85310228751642114 ) ) ;
#5778 = DIRECTION ( 'NONE',  ( 0.000000000000000000, -1.000000000000000000, 0.000000000000000000 ) ) ;
#5779 = CARTESIAN_POINT ( 'NONE',  ( -83.00000000000001421, 0.000000000000000000, 8.000000000000000000 ) ) ;
#5780 = CARTESIAN_POINT ( 'NONE',  ( -7.750357176954294935, 12.08964793087877787, 44.21024514465928235 ) ) ;
#5781 = CARTESIAN_POINT ( 'NONE',  ( 10.91227292449344155, 1.677562661911773390, 12.05113791807856671 ) ) ;
#5782 = CARTESIAN_POINT ( 'NONE',  ( -1.776620879821455556, -10.89658364409025992, 3.951137918078560851 ) ) ;
#5783 =( GEOMETRIC_REPRESENTATION_CONTEXT ( 3 ) GLOBAL_UNCERTAINTY_ASSIGNED_CONTEXT ( ( #3587 ) ) GLOBAL_UNIT_ASSIGNED_CONTEXT ( ( #7262, #1591, #5706 ) ) REPRESENTATION_CONTEXT ( 'NONE', 'WORKASPACE' ) );
#5784 = VECTOR ( 'NONE', #6807, 1000.000000000000000 ) ;
#5785 = CARTESIAN_POINT ( 'NONE',  ( -6.919986107680330178, -12.02850919814119557, -1.270000000000007123 ) ) ;
#5786 = CARTESIAN_POINT ( 'NONE',  ( 13.59724543428031573, 4.619798703722006294, 17.93261199819786711 ) ) ;
#5787 = FILL_AREA_STYLE_COLOUR ( '', #635 ) ;
#5788 = CARTESIAN_POINT ( 'NONE',  ( -7.806708723663830618, -7.806708723663901672, 11.24999999999999467 ) ) ;
#5789 = CARTESIAN_POINT ( 'NONE',  ( -11.51250119794888072, -11.69682198916848037, 42.49595943037355994 ) ) ;
#5790 = ORIENTED_EDGE ( 'NONE', *, *, #7151, .F. ) ;
#5791 = FACE_OUTER_BOUND ( 'NONE', #3445, .T. ) ;
#5792 = AXIS2_PLACEMENT_3D ( 'NONE', #5759, #5857, #5047 ) ;
#5793 = CARTESIAN_POINT ( 'NONE',  ( 13.47998361472151529, 8.620103694222146729, 9.710245144659278793 ) ) ;
#5794 = DIRECTION ( 'NONE',  ( -1.000000000000000000, -0.000000000000000000, -0.000000000000000000 ) ) ;
#5795 = CARTESIAN_POINT ( 'NONE',  ( -163.2908874445610365, -1.312003822475822146, 14.94297504947871325 ) ) ;
#5796 = CARTESIAN_POINT ( 'NONE',  ( -4.355403765523468529, -8.442910196168352144, 4.101137918078561206 ) ) ;
#5797 = CARTESIAN_POINT ( 'NONE',  ( 1.562606840307832368, 9.865911304835503159, 18.44999999999999218 ) ) ;
#5798 = DIRECTION ( 'NONE',  ( 1.000000000000000000, 4.755747939841215952E-17, -0.000000000000000000 ) ) ;
#5799 = CLOSED_SHELL ( 'NONE', ( #132, #9113, #7853, #4392, #401, #7617, #8610, #8088, #7234, #6359, #3871, #10214, #6977, #2579, #6225, #1146, #3895 ) ) ;
#5800 = CARTESIAN_POINT ( 'NONE',  ( -1.607813917173034124, 14.26974319298267524, 30.64285714285715301 ) ) ;
#5801 = ORIENTED_EDGE ( 'NONE', *, *, #8801, .T. ) ;
#5802 = CARTESIAN_POINT ( 'NONE',  ( -8.512513224245306986, -13.54758718765259218, 46.28571428571429180 ) ) ;
#5803 = CARTESIAN_POINT ( 'NONE',  ( 3.607533428936334552, 14.36432425738846419, -9.697396257098264345E-17 ) ) ;
#5804 = CARTESIAN_POINT ( 'NONE',  ( -8.731428362939189114, 13.89598863503036341, 18.21428571428571885 ) ) ;
#5805 = EDGE_CURVE ( 'NONE', #1309, #728, #6656, .T. ) ;
#5806 = DIRECTION ( 'NONE',  ( 0.000000000000000000, 0.000000000000000000, 1.000000000000000000 ) ) ;
#5807 = CARTESIAN_POINT ( 'NONE',  ( -4.579542530753125895, 8.877401133907090625, 16.14886208192145389 ) ) ;
#5808 = CARTESIAN_POINT ( 'NONE',  ( -6.751237864895158758, 6.683790977649255005, 3.998862081921419342 ) ) ;
#5809 = CARTESIAN_POINT ( 'NONE',  ( 16.29368510291089223, -1.967016585148476882, 12.36118342676929771 ) ) ;
#5810 = CARTESIAN_POINT ( 'NONE',  ( -16.30827793483735988, 1.837501619626141780, 23.35714285714286476 ) ) ;
#5811 = CARTESIAN_POINT ( 'NONE',  ( 5.164528828830335705, -15.14410076328347543, 7.432611998197861780 ) ) ;
#5812 = AXIS2_PLACEMENT_3D ( 'NONE', #2023, #5181, #9171 ) ;
#5813 = CARTESIAN_POINT ( 'NONE',  ( -10.15407889436378852, -10.15407889436390576, 16.50000000000000000 ) ) ;
#5814 = CARTESIAN_POINT ( 'NONE',  ( -163.3500000000000512, -1.734723475976807094E-15, 3.000000000000002665 ) ) ;
#5815 = CARTESIAN_POINT ( 'NONE',  ( -10.89658364409024749, -1.776620879821561472, 12.54886208192144004 ) ) ;
#5816 = VERTEX_POINT ( 'NONE', #428 ) ;
#5817 = EDGE_CURVE ( 'NONE', #8798, #1952, #47, .T. ) ;
#5818 = CARTESIAN_POINT ( 'NONE',  ( 4.623906867372411078, -13.21436662431711717, 15.42857142857143060 ) ) ;
#5819 = ORIENTED_EDGE ( 'NONE', *, *, #100, .F. ) ;
#5820 = CARTESIAN_POINT ( 'NONE',  ( 5.284464991282756152, -15.10213328493384743, 33.42857142857143060 ) ) ;
#5821 = CARTESIAN_POINT ( 'NONE',  ( 11.40355824106246985, -11.22385875690704538, 40.99595943037355994 ) ) ;
#5822 = CARTESIAN_POINT ( 'NONE',  ( -9.837026868206066865, 5.012215536711413399, 8.850000000000008527 ) ) ;
#5823 = PRODUCT_DEFINITION_SHAPE ( 'NONE', 'NONE',  #7569 ) ;
#5824 = CARTESIAN_POINT ( 'NONE',  ( 11.85413878919593422, 7.448449071214774619, 7.714285714285715301 ) ) ;
#5825 = CARTESIAN_POINT ( 'NONE',  ( -7.750357176954294935, 12.08964793087877787, 32.21024514465928235 ) ) ;
#5826 = LINE ( 'NONE', #10178, #1449 ) ;
#5827 = CARTESIAN_POINT ( 'NONE',  ( 1.595235446793586753, 13.94740710718646248, 48.73000000000003951 ) ) ;
#5828 = CARTESIAN_POINT ( 'NONE',  ( -4.743843029824828861, 13.17239914596749450, 38.42453085894499054 ) ) ;
#5829 = CARTESIAN_POINT ( 'NONE',  ( 4.967534682030706250, -9.859792900771036983, 12.65113791807859123 ) ) ;
#5830 = CARTESIAN_POINT ( 'NONE',  ( 10.36326688006723984, -1.689666864740212215, 3.201137918078536426 ) ) ;
#5831 = EDGE_CURVE ( 'NONE', #3923, #9360, #1046, .T. ) ;
#5832 = AXIS2_PLACEMENT_3D ( 'NONE', #10141, #2188, #1516 ) ;
#5833 = DIRECTION ( 'NONE',  ( 1.000000000000000000, 4.755747939841215952E-17, -0.000000000000000000 ) ) ;
#5834 = CARTESIAN_POINT ( 'NONE',  ( -13.17239914596754424, 4.743843029824683200, 27.57546914105500946 ) ) ;
#5835 = CARTESIAN_POINT ( 'NONE',  ( 4.766900247265192903, 9.355568503977911732, 6.599999999999994316 ) ) ;
#5836 = CARTESIAN_POINT ( 'NONE',  ( 13.47998361472151529, 8.620103694222146729, 33.71024514465927524 ) ) ;
#5837 = DIRECTION ( 'NONE',  ( -1.000000000000000000, -0.000000000000000000, -0.000000000000000000 ) ) ;
#5838 = CARTESIAN_POINT ( 'NONE',  ( -15.10213328493390961, 5.284464991282586510, 17.57142857142856940 ) ) ;
#5839 = CARTESIAN_POINT ( 'NONE',  ( -8.404922754268618235, -13.61519076058357491, 6.281673716087846415 ) ) ;
#5840 = DIRECTION ( 'NONE',  ( -1.000000000000000000, -0.000000000000000000, -0.000000000000000000 ) ) ;
#5841 = CARTESIAN_POINT ( 'NONE',  ( -7.098671581784199880, -7.027753727702804376, 10.25113791807858021 ) ) ;
#5842 = CARTESIAN_POINT ( 'NONE',  ( 4.312909747525650594, 8.464561979789532842, 12.59999999999999964 ) ) ;
#5843 = CARTESIAN_POINT ( 'NONE',  ( -165.5648848242107647, 2.093279044514479992, 14.85361548801915887 ) ) ;
#5844 = CARTESIAN_POINT ( 'NONE',  ( 13.61519076058348254, 8.404922754268771001, 35.71832628391214115 ) ) ;
#5845 = CARTESIAN_POINT ( 'NONE',  ( -10.15407889436378852, -10.15407889436390576, 34.50000000000000000 ) ) ;
#5846 = CARTESIAN_POINT ( 'NONE',  ( -10.15407889436378852, -10.15407889436390576, 34.50000000000000000 ) ) ;
#5847 = EDGE_LOOP ( 'NONE', ( #9564, #3247, #1834, #2406 ) ) ;
#5848 = CARTESIAN_POINT ( 'NONE',  ( 16.30827793483735633, -1.837501619626142890, 38.35714285714287541 ) ) ;
#5849 = DIRECTION ( 'NONE',  ( 1.000000000000000000, 0.000000000000000000, 0.000000000000000000 ) ) ;
#5850 = CARTESIAN_POINT ( 'NONE',  ( -11.31370849898482156, 11.31370849898469544, 18.00000000000000355 ) ) ;
#5851 = LINE ( 'NONE', #9028, #9265 ) ;
#5852 = CARTESIAN_POINT ( 'NONE',  ( 9.858066664633883036, 1.612135949262857526, 20.04886208192142050 ) ) ;
#5853 = CARTESIAN_POINT ( 'NONE',  ( 1.513077731352925115, 9.873755945037103743, 10.44886208192141908 ) ) ;
#5854 = UNCERTAINTY_MEASURE_WITH_UNIT (LENGTH_MEASURE( 1.000000000000000082E-05 ), #5086, 'distance_accuracy_value', 'NONE');
#5855 = CARTESIAN_POINT ( 'NONE',  ( -1.917699372585823570, -15.88516839912900558, 13.86118342676929416 ) ) ;
#5856 = CARTESIAN_POINT ( 'NONE',  ( 15.10213328493390783, -5.284464991282587398, 26.57142857142857295 ) ) ;
#5857 = DIRECTION ( 'NONE',  ( -1.000000000000000000, 0.000000000000000000, 0.000000000000000000 ) ) ;
#5858 = CARTESIAN_POINT ( 'NONE',  ( -8.621071003556675549, 13.96533075980314642, 4.218326283912150032 ) ) ;
#5859 = CARTESIAN_POINT ( 'NONE',  ( -11.85413878919593422, -7.448449071214776396, 22.71428571428571530 ) ) ;
#5860 = CARTESIAN_POINT ( 'NONE',  ( -11.60466159355861926, -11.60466159355875249, 10.50000000000000533 ) ) ;
#5861 = CARTESIAN_POINT ( 'NONE',  ( -5.056896391392315948, 9.814260835640997271, 10.14886208192142725 ) ) ;
#5862 = ORIENTED_EDGE ( 'NONE', *, *, #2378, .T. ) ;
#5863 = CARTESIAN_POINT ( 'NONE',  ( 4.742819248065503146, 13.55419868402813677, 19.07142857142856940 ) ) ;
#5864 = VERTEX_POINT ( 'NONE', #9888 ) ;
#5865 = CARTESIAN_POINT ( 'NONE',  ( 13.89598863503045933, -8.731428362939032795, 32.78571428571429180 ) ) ;
#5866 = CARTESIAN_POINT ( 'NONE',  ( -13.89774397934249706, -1.693770420379375974, 7.138816573230711171 ) ) ;
#5867 = CARTESIAN_POINT ( 'NONE',  ( 5.056896391392317724, -9.814260835640970626, 2.648862081921448119 ) ) ;
#5868 = APPLICATION_PROTOCOL_DEFINITION ( 'draft international standard', 'automotive_design', 1998, #7182 ) ;
#5869 = CARTESIAN_POINT ( 'NONE',  ( -13.91197093850538380, -1.567502665446387278, 17.14285714285713880 ) ) ;
#5870 = VECTOR ( 'NONE', #1057, 1000.000000000000000 ) ;
#5871 = ORIENTED_EDGE ( 'NONE', *, *, #6995, .F. ) ;
#5872 = CARTESIAN_POINT ( 'NONE',  ( -11.78653521626494793, -7.556039541191465148, 30.71024514465928235 ) ) ;
#5873 = ORIENTED_EDGE ( 'NONE', *, *, #6843, .T. ) ;
#5874 = CARTESIAN_POINT ( 'NONE',  ( -158.0000000000000284, -6.938893903907228378E-15, 0.000000000000000000 ) ) ;
#5875 = CARTESIAN_POINT ( 'NONE',  ( 3.470966000225593096, 13.60552200844329285, 48.73000000000002530 ) ) ;
#5876 = CARTESIAN_POINT ( 'NONE',  ( 9.333916720356675967, 4.809394265263126300, 16.89886208192141126 ) ) ;
#5877 = CARTESIAN_POINT ( 'NONE',  ( 11.85413878919593422, 7.448449071214774619, 1.714285714285716855 ) ) ;
#5878 = CARTESIAN_POINT ( 'NONE',  ( -10.91227292449344155, -1.677562661911749187, 10.55113791807857204 ) ) ;
#5879 = CARTESIAN_POINT ( 'NONE',  ( 7.842167650704563897, 7.771249796623202144, 2.751137918078555789 ) ) ;
#5880 = AXIS2_PLACEMENT_3D ( 'NONE', #7754, #7019, #5419 ) ;
#5881 = CARTESIAN_POINT ( 'NONE',  ( 2.000000000000001776, 0.8865213383407039016, -1.535500000000022958 ) ) ;
#5882 = CARTESIAN_POINT ( 'NONE',  ( -7.529642458189277576, 12.22833218042435455, 16.21832628391214470 ) ) ;
#5883 = CARTESIAN_POINT ( 'NONE',  ( 10.90442828429183919, 1.727091770866678422, 4.049999999999988276 ) ) ;
#5884 = CARTESIAN_POINT ( 'NONE',  ( 11.40355824106246985, -11.22385875690704538, 34.99595943037355994 ) ) ;
#5885 = CARTESIAN_POINT ( 'NONE',  ( -12.50678508136871869, 7.704882173211043295, 48.73000000000002530 ) ) ;
#5886 = CARTESIAN_POINT ( 'NONE',  ( -16.30827793483735988, 1.837501619626141780, 23.35714285714286476 ) ) ;
#5887 = CARTESIAN_POINT ( 'NONE',  ( 0.000000000000000000, 0.000000000000000000, -1.270000000000007123 ) ) ;
#5888 = CARTESIAN_POINT ( 'NONE',  ( 14.28433602490915000, -1.478298951650544479, 10.35310228751642292 ) ) ;
#5889 = CARTESIAN_POINT ( 'NONE',  ( 4.490180821391514421, -8.922933199037139218, 3.651137918078570355 ) ) ;
#5890 = CARTESIAN_POINT ( 'NONE',  ( 4.312909747525650594, 8.464561979789532842, 15.60000000000000320 ) ) ;
#5891 = CARTESIAN_POINT ( 'NONE',  ( -163.3795937461757433, 1.420165590446639259, 14.93295938614575036 ) ) ;
#5892 = CARTESIAN_POINT ( 'NONE',  ( -4.742819248065502258, -13.55419868402813677, 28.07142857142857295 ) ) ;
#5893 = EDGE_CURVE ( 'NONE', #9714, #8514, #5128, .T. ) ;
#5894 = CARTESIAN_POINT ( 'NONE',  ( 10.15407889436379030, 10.15407889436390576, 43.50000000000000711 ) ) ;
#5895 = ORIENTED_EDGE ( 'NONE', *, *, #6467, .F. ) ;
#5896 = AXIS2_PLACEMENT_3D ( 'NONE', #1079, #6577, #196 ) ;
#5897 = CARTESIAN_POINT ( 'NONE',  ( -1.837501619626328297, 16.30827793483733856, 48.64285714285716011 ) ) ;
#5898 = CARTESIAN_POINT ( 'NONE',  ( -17.72919999999999874, 2.171200803144325526E-15, -1.270000000000007123 ) ) ;
#5899 = CARTESIAN_POINT ( 'NONE',  ( 5.420364854932001819, 15.49051278174644430, 13.07142857142857295 ) ) ;
#5900 = DIRECTION ( 'NONE',  ( -1.000000000000000000, 0.000000000000000000, 0.000000000000000000 ) ) ;
#5901 = CARTESIAN_POINT ( 'NONE',  ( -168.0000000000000284, -2.363368035607170010E-15, 0.000000000000000000 ) ) ;
#5902 = PRODUCT_DEFINITION_SHAPE ( 'NONE', 'NONE',  #5604 ) ;
#5903 = CARTESIAN_POINT ( 'NONE',  ( -68.00000000000001421, 0.000000000000000000, 0.000000000000000000 ) ) ;
#5904 = CARTESIAN_POINT ( 'NONE',  ( 4.579542530753127672, -8.877401133907065756, 17.64886208192141126 ) ) ;
#5905 = CARTESIAN_POINT ( 'NONE',  ( -4.270415729527831772, -8.486213763410670907, 9.098862081921437195 ) ) ;
#5906 = CARTESIAN_POINT ( 'NONE',  ( -5.164528828830334817, 15.14410076328347543, 10.43261199819786356 ) ) ;
#5907 = CARTESIAN_POINT ( 'NONE',  ( -5.284464991282755264, 15.10213328493384743, 24.42857142857143060 ) ) ;
#5908 = EDGE_CURVE ( 'NONE', #4031, #3628, #5675, .T. ) ;
#5909 = CARTESIAN_POINT ( 'NONE',  ( -13.55419868402807992, -4.742819248065651472, 46.92857142857143060 ) ) ;
#5910 = CARTESIAN_POINT ( 'NONE',  ( 15.53355953199861794, 5.297344310588528060, 11.93261199819786178 ) ) ;
#5911 = EDGE_CURVE ( 'NONE', #3468, #7869, #7670, .T. ) ;
#5912 = CARTESIAN_POINT ( 'NONE',  ( -9.899494936611716867, 9.899494936611610285, 18.00000000000000355 ) ) ;
#5913 = CARTESIAN_POINT ( 'NONE',  ( 15.49051278174638036, 5.420364854932175014, 1.928571428571430380 ) ) ;
#5914 = CYLINDRICAL_SURFACE ( 'NONE', #6930, 8.200000000000001066 ) ;
#5915 = VERTEX_POINT ( 'NONE', #477 ) ;
#5916 = CARTESIAN_POINT ( 'NONE',  ( -4.742819248065502258, -13.55419868402813677, 16.07142857142857650 ) ) ;
#5917 = CARTESIAN_POINT ( 'NONE',  ( 15.49051278174637858, 5.420364854932174126, 31.92857142857143060 ) ) ;
#5918 = CARTESIAN_POINT ( 'NONE',  ( -5.297344310588352201, -15.53355953199867301, 48.06738800180213644 ) ) ;
#5919 = CARTESIAN_POINT ( 'NONE',  ( 7.771249796623105333, 7.842167650704658932, 1.748862081921432887 ) ) ;
#5920 = APPLICATION_PROTOCOL_DEFINITION ( 'draft international standard', 'automotive_design', 1998, #6245 ) ;
#5921 = CARTESIAN_POINT ( 'NONE',  ( 13.91197093850538380, 1.567502665446386390, 8.142857142857145902 ) ) ;
#5922 = ORIENTED_EDGE ( 'NONE', *, *, #6815, .T. ) ;
#5923 = CARTESIAN_POINT ( 'NONE',  ( -1.441234910513241818, -13.92619789766829008, 29.85310228751642470 ) ) ;
#5924 = VECTOR ( 'NONE', #3272, 1000.000000000000000 ) ;
#5925 = VERTEX_POINT ( 'NONE', #1464 ) ;
#5926 =( NAMED_UNIT ( * ) SI_UNIT ( $, .STERADIAN. ) SOLID_ANGLE_UNIT ( ) );
#5927 = CARTESIAN_POINT ( 'NONE',  ( -0.3021515714675195863, 13.99673906407701729, 48.73000000000003951 ) ) ;
#5928 = CARTESIAN_POINT ( 'NONE',  ( 9.390499931835536884, -1.439022436064273158, 2.198862081921450606 ) ) ;
#5929 = CARTESIAN_POINT ( 'NONE',  ( -13.51115193377584589, -4.865839792409295761, 48.92453085894499054 ) ) ;
#5930 = CARTESIAN_POINT ( 'NONE',  ( 4.766900247265192903, 9.355568503977911732, 6.599999999999994316 ) ) ;
#5931 = CARTESIAN_POINT ( 'NONE',  ( -7.842167650704559456, -7.771249796623176387, 7.251137918078588207 ) ) ;
#5932 = DIRECTION ( 'NONE',  ( 0.000000000000000000, 1.000000000000000000, -9.714451465470119729E-16 ) ) ;
#5933 = CARTESIAN_POINT ( 'NONE',  ( 4.503970704919991519, -13.25633410266674517, 31.43261199819787421 ) ) ;
#5934 = AXIS2_PLACEMENT_3D ( 'NONE', #9026, #1937, #9131 ) ;
#5935 = CARTESIAN_POINT ( 'NONE',  ( -5.012215536711506658, 9.837026868206022456, 6.149999999999980815 ) ) ;
#5936 = CARTESIAN_POINT ( 'NONE',  ( -1.967016585148659846, 16.29368510291087091, 44.63881657323071295 ) ) ;
#5937 = CARTESIAN_POINT ( 'NONE',  ( -12.62058114252586805, 7.581620562087779014, 48.73000000000001108 ) ) ;
#5938 = CARTESIAN_POINT ( 'NONE',  ( -8.731428362939189114, 13.89598863503036341, 18.21428571428571885 ) ) ;
#5939 = DIRECTION ( 'NONE',  ( 0.000000000000000000, -8.191099868251446680E-34, -1.000000000000000000 ) ) ;
#5940 = VECTOR ( 'NONE', #9447, 1000.000000000000114 ) ;
#5941 = AXIS2_PLACEMENT_3D ( 'NONE', #3565, #7496, #1871 ) ;
#5942 = CARTESIAN_POINT ( 'NONE',  ( -4.619798703721853528, -13.59724543428036725, 12.06738800180214000 ) ) ;
#5943 = CARTESIAN_POINT ( 'NONE',  ( 4.490180821391514421, -8.922933199037132113, 12.65113791807859123 ) ) ;
#5944 = CARTESIAN_POINT ( 'NONE',  ( -6.683790977649319842, 6.751237864895101026, -0.9988620819214586444 ) ) ;
#5945 = CARTESIAN_POINT ( 'NONE',  ( -164.7177004374966032, 2.136022552468798796, 14.84716063139783593 ) ) ;
#5946 = CARTESIAN_POINT ( 'NONE',  ( -15.06016580658428694, 5.404401153735006957, 33.57546914105500946 ) ) ;
#5947 = CARTESIAN_POINT ( 'NONE',  ( -1.607813917173034124, 14.26974319298267524, 48.64285714285716011 ) ) ;
#5948 = STYLED_ITEM ( 'NONE', ( #9762 ), #9686 ) ;
#5949 = CARTESIAN_POINT ( 'NONE',  ( 12.15899005565164792, -7.639999817571655250, 38.78571428571429180 ) ) ;
#5950 = VERTEX_POINT ( 'NONE', #2949 ) ;
#5951 = CARTESIAN_POINT ( 'NONE',  ( -11.31370849898482156, 11.31370849898469544, 42.00000000000000000 ) ) ;
#5952 = DIRECTION ( 'NONE',  ( -4.755747939841215952E-17, 1.000000000000000000, 0.000000000000000000 ) ) ;
#5953 = CARTESIAN_POINT ( 'NONE',  ( -8.731428362939189114, 13.89598863503036341, 24.21428571428571530 ) ) ;
#5954 = CARTESIAN_POINT ( 'NONE',  ( -58.00000000000002842, 1.501835218140774790E-15, -13.00000000000001243 ) ) ;
#5955 = DIRECTION ( 'NONE',  ( -1.000000000000000000, -0.000000000000000000, -0.000000000000000000 ) ) ;
#5956 = CARTESIAN_POINT ( 'NONE',  ( -4.312909747525649706, -8.464561979789507973, 5.099999999999993427 ) ) ;
#5957 = CARTESIAN_POINT ( 'NONE',  ( 4.579542530753127672, -8.877401133907065756, 11.64886208192146988 ) ) ;
#5958 = UNCERTAINTY_MEASURE_WITH_UNIT (LENGTH_MEASURE( 1.000000000000000082E-05 ), #1611, 'distance_accuracy_value', 'NONE');
#5959 = CARTESIAN_POINT ( 'NONE',  ( 9.355568503977840678, 4.766900247265305701, 15.90000000000002522 ) ) ;
#5960 = CARTESIAN_POINT ( 'NONE',  ( 15.53355953199861794, 5.297344310588528060, 11.93261199819786178 ) ) ;
#5961 = CARTESIAN_POINT ( 'NONE',  ( 11.60466159355862104, 11.60466159355875071, 31.50000000000001421 ) ) ;
#5962 = SHAPE_REPRESENTATION_RELATIONSHIP ( 'NONE' , 'NONE' ,  #789, #9686 ) ;
#5963 = CARTESIAN_POINT ( 'NONE',  ( 15.06016580658428694, -5.404401153735007846, 6.575469141055007682 ) ) ;
#5964 = CARTESIAN_POINT ( 'NONE',  ( 13.21436662431716869, -4.623906867372263640, 20.57142857142857295 ) ) ;
#5965 = CARTESIAN_POINT ( 'NONE',  ( -1.837501619626328297, 16.30827793483733856, 6.642857142857143238 ) ) ;
#5966 = CARTESIAN_POINT ( 'NONE',  ( 15.49051278174638036, 5.420364854932175014, 43.92857142857143060 ) ) ;
#5967 = ORIENTED_EDGE ( 'NONE', *, *, #8032, .T. ) ;
#5968 = CARTESIAN_POINT ( 'NONE',  ( -10.90442828429183919, -1.727091770866654663, 17.55000000000002913 ) ) ;
#5969 = ORIENTED_EDGE ( 'NONE', *, *, #6565, .F. ) ;
#5970 = CARTESIAN_POINT ( 'NONE',  ( 13.89598863503045933, -8.731428362939032795, 26.78571428571429180 ) ) ;
#5971 = CARTESIAN_POINT ( 'NONE',  ( 5.297344310588354865, 15.53355953199867301, 51.06738800180214355 ) ) ;
#5972 = CARTESIAN_POINT ( 'NONE',  ( -9.837026868206066865, 5.012215536711413399, 14.84999999999999787 ) ) ;
#5973 = APPLICATION_PROTOCOL_DEFINITION ( 'draft international standard', 'automotive_design', 1998, #4679 ) ;
#5974 = CARTESIAN_POINT ( 'NONE',  ( 1.567502665446232957, 13.91197093850540156, 30.85714285714286120 ) ) ;
#5975 = EDGE_CURVE ( 'NONE', #7869, #3468, #2359, .T. ) ;
#5976 = CARTESIAN_POINT ( 'NONE',  ( -7.340858601237953529, -11.92174236212700222, 30.28167371608785530 ) ) ;
#5977 = VERTEX_POINT ( 'NONE', #3842 ) ;
#5978 = CARTESIAN_POINT ( 'NONE',  ( 6.976602070941136269, -13.58603705635637304, 0.000000000000000000 ) ) ;
#5979 = DIRECTION ( 'NONE',  ( -1.000000000000000000, -0.000000000000000000, -0.000000000000000000 ) ) ;
#5980 = CARTESIAN_POINT ( 'NONE',  ( 5.056896391392317724, -9.814260835640970626, 17.64886208192141126 ) ) ;
#5981 = CARTESIAN_POINT ( 'NONE',  ( -1.567502665446231180, -13.91197093850540334, 3.857142857142857650 ) ) ;
#5982 = CARTESIAN_POINT ( 'NONE',  ( -10.90442828429183919, -1.727091770866655329, 8.549999999999963407 ) ) ;
#5983 = CARTESIAN_POINT ( 'NONE',  ( -7.390897758835869524, 7.458344646081637386, 14.00113791807859620 ) ) ;
#5984 = FACE_OUTER_BOUND ( 'NONE', #9322, .T. ) ;
#5985 = CARTESIAN_POINT ( 'NONE',  ( 10.24623928997352884, 10.06191849875416899, 29.50404056962643295 ) ) ;
#5986 = CARTESIAN_POINT ( 'NONE',  ( 7.424621202458790314, -7.424621202458697944, 4.500000000000003553 ) ) ;
#5987 = CARTESIAN_POINT ( 'NONE',  ( -15.44746603149413922, -5.543385399275820191, 36.92453085894499765 ) ) ;
#5988 = ORIENTED_EDGE ( 'NONE', *, *, #8921, .F. ) ;
#5989 = CARTESIAN_POINT ( 'NONE',  ( -12.79983919530466707, 7.405287656185944201, 48.73000000000000398 ) ) ;
#5990 = CARTESIAN_POINT ( 'NONE',  ( -16.30827793483735988, 1.837501619626141780, 29.35714285714285765 ) ) ;
#5991 = DIRECTION ( 'NONE',  ( 0.000000000000000000, 0.000000000000000000, 1.000000000000000000 ) ) ;
#5992 = VECTOR ( 'NONE', #6643, 1000.000000000000000 ) ;
#5993 = CARTESIAN_POINT ( 'NONE',  ( -11.78653521626494793, -7.556039541191465148, 12.71024514465927879 ) ) ;
#5994 = CARTESIAN_POINT ( 'NONE',  ( -1.439022436064386845, 9.390499931835535108, 17.30113791807856316 ) ) ;
#5995 = CARTESIAN_POINT ( 'NONE',  ( 8.464561979789474222, 4.312909747525755400, 12.90000000000002345 ) ) ;
#5996 = FACE_OUTER_BOUND ( 'NONE', #7743, .T. ) ;
#5997 = CARTESIAN_POINT ( 'NONE',  ( 11.85413878919593422, 7.448449071214774619, 43.71428571428572241 ) ) ;
#5998 = CARTESIAN_POINT ( 'NONE',  ( -12.15899005565164792, 7.639999817571651697, 41.78571428571430602 ) ) ;
#5999 = EDGE_LOOP ( 'NONE', ( #7068, #8364, #9837, #607 ) ) ;
#6000 = CARTESIAN_POINT ( 'NONE',  ( 8.731428362939190890, -13.89598863503036164, 39.21428571428571530 ) ) ;
#6001 = DIRECTION ( 'NONE',  ( 1.000000000000000000, 4.755747939841215952E-17, -0.000000000000000000 ) ) ;
#6002 = CARTESIAN_POINT ( 'NONE',  ( 15.89939535829187278, 1.791431617653015174, 32.14285714285714590 ) ) ;
#6003 = CARTESIAN_POINT ( 'NONE',  ( 2.000000000000001776, -0.8865213383406761460, 1.535499999999911935 ) ) ;
#6004 = CARTESIAN_POINT ( 'NONE',  ( -4.246973736992222470, -14.10948682827616096, 0.000000000000000000 ) ) ;
#6005 = EDGE_CURVE ( 'NONE', #10061, #6421, #4534, .T. ) ;
#6006 = PLANE ( 'NONE',  #842 ) ;
#6007 = CARTESIAN_POINT ( 'NONE',  ( -4.312909747525649706, -8.464561979789499091, 8.099999999999996092 ) ) ;
#6008 = CARTESIAN_POINT ( 'NONE',  ( -8.442910196168309511, -4.355403765523546689, 9.398862081921404155 ) ) ;
#6009 = CARTESIAN_POINT ( 'NONE',  ( 7.424621202458790314, -7.424621202458697944, 16.50000000000001421 ) ) ;
#6010 = CARTESIAN_POINT ( 'NONE',  ( 5.284464991282756152, -15.10213328493384743, 39.42857142857143060 ) ) ;
#6011 = CARTESIAN_POINT ( 'NONE',  ( 13.61519076058348254, 8.404922754268771001, 23.71832628391215181 ) ) ;
#6012 = CARTESIAN_POINT ( 'NONE',  ( -1.567502665446231180, -13.91197093850540334, 27.85714285714285765 ) ) ;
#6013 = CARTESIAN_POINT ( 'NONE',  ( -1.837501619626328297, 16.30827793483733856, 0.6428571428571432378 ) ) ;
#6014 = CARTESIAN_POINT ( 'NONE',  ( -1.837501619626328297, 16.30827793483733856, 42.64285714285715301 ) ) ;
#6015 = ORIENTED_EDGE ( 'NONE', *, *, #4161, .T. ) ;
#6016 = CARTESIAN_POINT ( 'NONE',  ( -9.837026868206066865, 5.012215536711416064, 11.84999999999997478 ) ) ;
#6017 = ORIENTED_EDGE ( 'NONE', *, *, #4876, .F. ) ;
#6018 = CARTESIAN_POINT ( 'NONE',  ( -8.512513224245306986, -13.54758718765259218, 40.28571428571428470 ) ) ;
#6019 = CARTESIAN_POINT ( 'NONE',  ( 7.750357176954296712, -12.08964793087877787, 5.210245144659280569 ) ) ;
#6020 = CARTESIAN_POINT ( 'NONE',  ( -7.458344646081709328, 7.390897758835804687, 0.9988620819214170110 ) ) ;
#6021 = CARTESIAN_POINT ( 'NONE',  ( -5.284464991282755264, 15.10213328493384743, 6.428571428571429713 ) ) ;
#6022 = CARTESIAN_POINT ( 'NONE',  ( 9.899494936611718643, -9.899494936611608509, 27.00000000000000355 ) ) ;
#6023 = EDGE_CURVE ( 'NONE', #2493, #5109, #8152, .T. ) ;
#6024 = CARTESIAN_POINT ( 'NONE',  ( 10.06191849875406064, 10.24623928997363187, 39.49595943037357415 ) ) ;
#6025 = ORIENTED_EDGE ( 'NONE', *, *, #7934, .T. ) ;
#6026 = CYLINDRICAL_SURFACE ( 'NONE', #9864, 1.816100000000000270 ) ;
#6027 = CARTESIAN_POINT ( 'NONE',  ( 15.44746603149413922, 5.543385399275817527, 27.92453085894499054 ) ) ;
#6028 = DIRECTION ( 'NONE',  ( -1.000000000000000000, 1.842239752758738928E-31, -1.780435181894459419E-32 ) ) ;
#6029 = CARTESIAN_POINT ( 'NONE',  ( 1.677562661911645714, 10.91227292449347175, 19.44886208192144039 ) ) ;
#6030 = CARTESIAN_POINT ( 'NONE',  ( 4.766900247265192903, 9.355568503977911732, 9.599999999999997868 ) ) ;
#6031 = CARTESIAN_POINT ( 'NONE',  ( 4.809394265263009061, 9.333916720356734587, 11.60113791807856742 ) ) ;
#6032 = CARTESIAN_POINT ( 'NONE',  ( -108.0000000000000426, 0.000000000000000000, 0.000000000000000000 ) ) ;
#6033 = CARTESIAN_POINT ( 'NONE',  ( -12.08964793087886314, 7.750357176954159932, 33.78975485534073897 ) ) ;
#6034 = EDGE_CURVE ( 'NONE', #1705, #7728, #6992, .T. ) ;
#6035 = ORIENTED_EDGE ( 'NONE', *, *, #769, .F. ) ;
#6036 = PRODUCT_DEFINITION ( 'UNKNOWN', '', #9058, #8984 ) ;
#6037 = CARTESIAN_POINT ( 'NONE',  ( 7.424621202458790314, -7.424621202458697944, 19.50000000000001776 ) ) ;
#6038 = CARTESIAN_POINT ( 'NONE',  ( -16.32287076676382398, 1.707986654103809343, 49.35310228751642114 ) ) ;
#6039 = CARTESIAN_POINT ( 'NONE',  ( -12.86610055725239654, 8.450849116819570739, 48.72999999999998977 ) ) ;
#6040 = CARTESIAN_POINT ( 'NONE',  ( 0.000000000000000000, 1.773042676681366281, 0.000000000000000000 ) ) ;
#6041 = CARTESIAN_POINT ( 'NONE',  ( 12.22833218042443271, -7.529642458189144349, 22.78167371608784464 ) ) ;
#6042 = CARTESIAN_POINT ( 'NONE',  ( 8.877401133907127928, -4.579542530753017537, 18.35113791807858519 ) ) ;
#6043 = CARTESIAN_POINT ( 'NONE',  ( 4.355403765523470305, 8.442910196168369907, 8.601137918078563871 ) ) ;
#6044 = CARTESIAN_POINT ( 'NONE',  ( -167.1500000000000341, -5.483569848023176209E-15, 13.00000000000000178 ) ) ;
#6045 = APPLICATION_CONTEXT ( 'automotive_design' ) ;
#6046 = CARTESIAN_POINT ( 'NONE',  ( 16.29368510291089223, -1.967016585148476882, 42.36118342676930126 ) ) ;
#6047 = CARTESIAN_POINT ( 'NONE',  ( 11.85413878919593422, 7.448449071214774619, 37.71428571428571530 ) ) ;
#6048 = CARTESIAN_POINT ( 'NONE',  ( 11.92174236212692229, 7.340858601238088532, 5.718326283912152697 ) ) ;
#6049 = ORIENTED_EDGE ( 'NONE', *, *, #5504, .T. ) ;
#6050 = CARTESIAN_POINT ( 'NONE',  ( 1.872357960115197173, 15.39586052177234521, -2.187087473825155240E-16 ) ) ;
#6051 = CARTESIAN_POINT ( 'NONE',  ( 16.30827793483735633, -1.837501619626142890, 32.35714285714286120 ) ) ;
#6052 = LINE ( 'NONE', #5954, #203 ) ;
#6053 = DIRECTION ( 'NONE',  ( 0.000000000000000000, 0.000000000000000000, 1.000000000000000000 ) ) ;
#6054 = CYLINDRICAL_SURFACE ( 'NONE', #4144, 18.00000000000000355 ) ;
#6055 = CARTESIAN_POINT ( 'NONE',  ( 1.486127417882244783, -9.383039235653791721, 4.800000000000026468 ) ) ;
#6056 = CARTESIAN_POINT ( 'NONE',  ( 4.312909747525650594, 8.464561979789532842, 0.5999999999999894307 ) ) ;
#6057 = CARTESIAN_POINT ( 'NONE',  ( -9.837026868206066865, 5.012215536711416064, 11.84999999999997478 ) ) ;
#6058 = EDGE_CURVE ( 'NONE', #6270, #4085, #3160, .T. ) ;
#6059 = CARTESIAN_POINT ( 'NONE',  ( 1.791431617652837316, 15.89939535829188877, 48.85714285714286120 ) ) ;
#6060 = ADVANCED_FACE ( 'NONE', ( #743 ), #7862, .T. ) ;
#6061 = AXIS2_PLACEMENT_3D ( 'NONE', #2916, #5299, #658 ) ;
#6062 = CARTESIAN_POINT ( 'NONE',  ( -5.543385399275643444, -15.44746603149420494, 14.07546914105500768 ) ) ;
#6063 = CARTESIAN_POINT ( 'NONE',  ( -7.448449071214644945, -11.85413878919601771, 28.28571428571428825 ) ) ;
#6064 = CARTESIAN_POINT ( 'NONE',  ( -15.10213328493390961, 5.284464991282586510, 5.571428571428574728 ) ) ;
#6065 = CARTESIAN_POINT ( 'NONE',  ( -11.31370849898482156, 11.31370849898469544, 42.00000000000000000 ) ) ;
#6066 = ORIENTED_EDGE ( 'NONE', *, *, #231, .T. ) ;
#6067 = CARTESIAN_POINT ( 'NONE',  ( 7.806708723663831506, 7.806708723663930982, 12.75000000000000533 ) ) ;
#6068 = ORIENTED_EDGE ( 'NONE', *, *, #2126, .F. ) ;
#6069 = CARTESIAN_POINT ( 'NONE',  ( -1.791431617652833763, -15.89939535829188877, 39.85714285714286120 ) ) ;
#6070 = CARTESIAN_POINT ( 'NONE',  ( -4.743843029824828861, 13.17239914596749450, 8.424530858944992318 ) ) ;
#6071 = CARTESIAN_POINT ( 'NONE',  ( 10.89658364409024749, 1.776620879821585897, 2.048862081921423162 ) ) ;
#6072 = CARTESIAN_POINT ( 'NONE',  ( 11.31370849898482334, -11.31370849898469366, 3.000000000000002665 ) ) ;
#6073 = CARTESIAN_POINT ( 'NONE',  ( 11.40355824106234550, 11.22385875690717327, 47.50404056962644006 ) ) ;
#6074 = CARTESIAN_POINT ( 'NONE',  ( 4.742819248065502258, 13.55419868402813499, 19.07142857142856940 ) ) ;
#6075 = CARTESIAN_POINT ( 'NONE',  ( -4.503970704919988854, 13.25633410266674517, 22.43261199819786356 ) ) ;
#6076 = CARTESIAN_POINT ( 'NONE',  ( 4.743843029824831525, -13.17239914596749095, 41.42453085894499765 ) ) ;
#6077 = EDGE_LOOP ( 'NONE', ( #6490, #3607, #902 ) ) ;
#6078 = FACE_OUTER_BOUND ( 'NONE', #9586, .T. ) ;
#6079 = CARTESIAN_POINT ( 'NONE',  ( -1.665163862719845067, -15.91362231745477374, 29.85310228751642470 ) ) ;
#6080 = CARTESIAN_POINT ( 'NONE',  ( -1.837501619626327853, 16.30827793483733856, 0.6428571428571433488 ) ) ;
#6081 = ADVANCED_FACE ( 'NONE', ( #3938 ), #737, .T. ) ;
#6082 = CARTESIAN_POINT ( 'NONE',  ( 1.689666864740335894, -10.36326688006720786, 17.79886208192143471 ) ) ;
#6083 = CARTESIAN_POINT ( 'NONE',  ( 7.750357176954296712, -12.08964793087877787, 47.21024514465928235 ) ) ;
#6084 = CARTESIAN_POINT ( 'NONE',  ( -10.90442828429183919, -1.727091770866654663, 2.550000000000035350 ) ) ;
#6085 = CARTESIAN_POINT ( 'NONE',  ( 10.36326688006723984, -1.689666864740210883, 18.20113791807854398 ) ) ;
#6086 = DIRECTION ( 'NONE',  ( 1.000000000000000000, 0.000000000000000000, 0.000000000000000000 ) ) ;
#6087 = CARTESIAN_POINT ( 'NONE',  ( 4.503970704919991519, -13.25633410266674517, 25.43261199819786711 ) ) ;
#6088 = EDGE_CURVE ( 'NONE', #5319, #2935, #9272, .T. ) ;
#6089 = MECHANICAL_DESIGN_GEOMETRIC_PRESENTATION_REPRESENTATION (  '', ( #1028 ), #1679 ) ;
#6090 = ORIENTED_EDGE ( 'NONE', *, *, #4728, .T. ) ;
#6091 = CARTESIAN_POINT ( 'NONE',  ( -5.297344310588352201, -15.53355953199867301, 48.06738800180213644 ) ) ;
#6092 = CARTESIAN_POINT ( 'NONE',  ( 1.642561882922480621, -10.37072757624892638, 1.800000000000023803 ) ) ;
#6093 = DIRECTION ( 'NONE',  ( 0.000000000000000000, -1.000000000000000000, 0.000000000000000000 ) ) ;
#6094 = CARTESIAN_POINT ( 'NONE',  ( -13.89774397934249706, -1.693770420379375974, 13.13881657323070584 ) ) ;
#6095 = CARTESIAN_POINT ( 'NONE',  ( 8.486213763410640709, 4.270415729527937465, 17.90113791807857524 ) ) ;
#6097 = VECTOR ( 'NONE', #4899, 999.9999999999998863 ) ;
#6096 = CARTESIAN_POINT ( 'NONE',  ( 8.486213763410640709, 4.270415729527937465, 8.901137918078571687 ) ) ;
#6098 = CIRCLE ( 'NONE', #508, 0.2000000000000000944 ) ;
#6099 = CARTESIAN_POINT ( 'NONE',  ( -163.9212390029829578, -1.865053163018561833, 12.86575946079389787 ) ) ;
#6100 = CARTESIAN_POINT ( 'NONE',  ( -11.69682198916834892, -11.51250119794901394, 44.50404056962644006 ) ) ;
#6101 = CARTESIAN_POINT ( 'NONE',  ( -7.639999817571787588, 12.15899005565156266, 42.21428571428572241 ) ) ;
#6102 = CARTESIAN_POINT ( 'NONE',  ( -11.92174236212692051, -7.340858601238089420, 2.718326283912150476 ) ) ;
#6103 = ORIENTED_EDGE ( 'NONE', *, *, #7927, .T. ) ;
#6104 = AXIS2_PLACEMENT_3D ( 'NONE', #1949, #5098, #8248 ) ;
#6105 = CARTESIAN_POINT ( 'NONE',  ( -13.47998361472151174, -8.620103694222146729, 6.710245144659284122 ) ) ;
#6106 = AXIS2_PLACEMENT_3D ( 'NONE', #26, #1534, #3180 ) ;
#6107 = CARTESIAN_POINT ( 'NONE',  ( 4.200000000000009059, 2.449293598294707893E-16, -2.000000000000000888 ) ) ;
#6108 = AXIS2_PLACEMENT_3D ( 'NONE', #9263, #6086, #2279 ) ;
#6109 = CARTESIAN_POINT ( 'NONE',  ( 5.284464991282756152, -15.10213328493384743, 27.42857142857143060 ) ) ;
#6110 = DIRECTION ( 'NONE',  ( 1.000000000000000000, 0.000000000000000000, 0.000000000000000000 ) ) ;
#6111 = CARTESIAN_POINT ( 'NONE',  ( 4.000000000000007105, 2.694222958124178486E-16, 2.200000000000001066 ) ) ;
#6112 = CARTESIAN_POINT ( 'NONE',  ( -9.865911304835474738, -1.562606840307925626, 11.54999999999998295 ) ) ;
#6113 = CARTESIAN_POINT ( 'NONE',  ( 7.027753727702739539, 7.098671581784288698, 16.74886208192143755 ) ) ;
#6114 = CARTESIAN_POINT ( 'NONE',  ( 0.2000000000000057288, 0.000000000000000000, 0.000000000000000000 ) ) ;
#6115 = CARTESIAN_POINT ( 'NONE',  ( -8.621071003556675549, 13.96533075980314642, 22.21832628391215181 ) ) ;
#6116 = CARTESIAN_POINT ( 'NONE',  ( 8.512513224245308763, 13.54758718765259040, 49.28571428571428470 ) ) ;
#6117 = CIRCLE ( 'NONE', #6602, 13.00000000000001066 ) ;
#6118 =( GEOMETRIC_REPRESENTATION_CONTEXT ( 3 ) GLOBAL_UNCERTAINTY_ASSIGNED_CONTEXT ( ( #9704 ) ) GLOBAL_UNIT_ASSIGNED_CONTEXT ( ( #5689, #8810, #270 ) ) REPRESENTATION_CONTEXT ( 'NONE', 'WORKASPACE' ) );
#6119 = CARTESIAN_POINT ( 'NONE',  ( -13.61519076058348254, -8.404922754268771001, 14.71832628391215003 ) ) ;
#6120 = ORIENTED_EDGE ( 'NONE', *, *, #6565, .T. ) ;
#6121 = CARTESIAN_POINT ( 'NONE',  ( -11.31370849898482156, 11.31370849898469544, 18.00000000000000355 ) ) ;
#6122 = CARTESIAN_POINT ( 'NONE',  ( 10.35987736339271770, 11.82290011998975388, 48.73000000000001819 ) ) ;
#6123 = FACE_OUTER_BOUND ( 'NONE', #9767, .T. ) ;
#6124 = CARTESIAN_POINT ( 'NONE',  ( 2.000000000000001776, 0.000000000000000000, 0.000000000000000000 ) ) ;
#6125 = COLOUR_RGB ( '', 0.66274510, 0.83137255, 0.94901961) ;
#6126 = CARTESIAN_POINT ( 'NONE',  ( -1.837501619626327853, 16.30827793483733856, 42.64285714285714590 ) ) ;
#6127 = CARTESIAN_POINT ( 'NONE',  ( 0.000000000000000000, 0.000000000000000000, 0.000000000000000000 ) ) ;
#6128 = CARTESIAN_POINT ( 'NONE',  ( 5.056896391392317724, -9.814260835640970626, 11.64886208192146988 ) ) ;
#6129 = CARTESIAN_POINT ( 'NONE',  ( -15.49051278174638036, -5.420364854932175902, 4.928571428571430602 ) ) ;
#6130 = CARTESIAN_POINT ( 'NONE',  ( 14.26974319298268767, -1.607813917172876472, 26.35714285714286120 ) ) ;
#6131 = ADVANCED_FACE ( 'NONE', ( #10193 ), #8694, .T. ) ;
#6132 = CARTESIAN_POINT ( 'NONE',  ( -7.063212654743467489, -7.063212654743533214, 5.250000000000008882 ) ) ;
#6133 = CARTESIAN_POINT ( 'NONE',  ( -10.06191849875405531, -10.24623928997363542, 36.49595943037355994 ) ) ;
#6134 = ORIENTED_EDGE ( 'NONE', *, *, #740, .T. ) ;
#6135 = DIRECTION ( 'NONE',  ( -0.000000000000000000, -0.000000000000000000, -1.000000000000000000 ) ) ;
#6136 = CARTESIAN_POINT ( 'NONE',  ( -11.40355824106246807, 11.22385875690704715, 25.99595943037356349 ) ) ;
#6137 = CARTESIAN_POINT ( 'NONE',  ( -11.60466159355861748, -11.60466159355874893, 4.500000000000003553 ) ) ;
#6138 = CARTESIAN_POINT ( 'NONE',  ( -1.513077731352923339, -9.873755945037078874, 5.948862081921430622 ) ) ;
#6139 = CARTESIAN_POINT ( 'NONE',  ( -8.841785722321695573, 13.82664651025757152, 20.21024514465928235 ) ) ;
#6140 = CARTESIAN_POINT ( 'NONE',  ( 5.110041130070070992, -16.97680807127747826, 0.000000000000000000 ) ) ;
#6141 = CARTESIAN_POINT ( 'NONE',  ( 9.377220287599001836, 4.724406229267489543, 17.90113791807857524 ) ) ;
#6142 = PLANE ( 'NONE',  #6594 ) ;
#6143 = CARTESIAN_POINT ( 'NONE',  ( 1.693770420379222319, 13.89774397934251837, 28.86118342676929416 ) ) ;
#6144 = VECTOR ( 'NONE', #9644, 1000.000000000000000 ) ;
#6145 = CARTESIAN_POINT ( 'NONE',  ( -4.743843029824828861, 13.17239914596749450, 2.424530858944988321 ) ) ;
#6146 = CARTESIAN_POINT ( 'NONE',  ( -10.90442828429184274, -1.727091770866655773, 5.549999999999998934 ) ) ;
#6147 = CARTESIAN_POINT ( 'NONE',  ( 8.512513224245308763, 13.54758718765259040, 31.28571428571428470 ) ) ;
#6148 = CARTESIAN_POINT ( 'NONE',  ( -68.00000000000001421, 0.000000000000000000, 0.000000000000000000 ) ) ;
#6149 = CIRCLE ( 'NONE', #1716, 13.00000000000000178 ) ;
#6150 = CARTESIAN_POINT ( 'NONE',  ( 7.750357176954296712, -12.08964793087877787, 29.21024514465927879 ) ) ;
#6151 = CARTESIAN_POINT ( 'NONE',  ( -7.098671581784199880, -7.027753727702809705, 13.25113791807857311 ) ) ;
#6152 = CARTESIAN_POINT ( 'NONE',  ( -4.490180821391513533, 8.922933199037158758, 8.151137918078559252 ) ) ;
#6153 = DIRECTION ( 'NONE',  ( 1.000000000000000000, 0.000000000000000000, 0.000000000000000000 ) ) ;
#6154 = CARTESIAN_POINT ( 'NONE',  ( -1.567502665446231180, -13.91197093850540334, 45.85714285714286120 ) ) ;
#6155 = CARTESIAN_POINT ( 'NONE',  ( -13.55419868402807992, -4.742819248065651472, 46.92857142857142350 ) ) ;
#6156 = VERTEX_POINT ( 'NONE', #6980 ) ;
#6157 = CARTESIAN_POINT ( 'NONE',  ( -1.665163862719845067, -15.91362231745477374, 5.853102287516418478 ) ) ;
#6158 = DIRECTION ( 'NONE',  ( -1.000000000000000000, -0.000000000000000000, -0.000000000000000000 ) ) ;
#6159 = CARTESIAN_POINT ( 'NONE',  ( 11.60466159355862104, 11.60466159355875071, 31.50000000000001421 ) ) ;
#6160 = AXIS2_PLACEMENT_3D ( 'NONE', #2235, #9325, #3889 ) ;
#6161 = DIRECTION ( 'NONE',  ( 1.000000000000000000, 0.000000000000000000, 0.000000000000000000 ) ) ;
#6162 = CARTESIAN_POINT ( 'NONE',  ( 0.000000000000000000, 0.000000000000000000, 0.000000000000000000 ) ) ;
#6163 = CARTESIAN_POINT ( 'NONE',  ( 4.766900247265192903, 9.355568503977902850, 0.5999999999999894307 ) ) ;
#6164 = CARTESIAN_POINT ( 'NONE',  ( -7.063212654743466601, -7.063212654743531438, 5.250000000000008882 ) ) ;
#6165 = CARTESIAN_POINT ( 'NONE',  ( -4.270415729527831772, -8.486213763410670907, 18.09886208192144252 ) ) ;
#6166 = DIRECTION ( 'NONE',  ( 1.000000000000000000, 0.000000000000000000, 0.000000000000000000 ) ) ;
#6167 = CARTESIAN_POINT ( 'NONE',  ( -8.731428362939189114, 13.89598863503036341, 42.21428571428572241 ) ) ;
#6168 = PRESENTATION_STYLE_ASSIGNMENT (( #3026 ) ) ;
#6169 = CARTESIAN_POINT ( 'NONE',  ( 11.22385875690717683, -11.40355824106234373, 25.00404056962644006 ) ) ;
#6170 = CARTESIAN_POINT ( 'NONE',  ( 9.563412070810842991, 12.55071356310834219, 48.73000000000002530 ) ) ;
#6171 = PRODUCT_RELATED_PRODUCT_CATEGORY ( 'part', '', ( #3525 ) ) ;
#6172 = CARTESIAN_POINT ( 'NONE',  ( -4.766900247265192014, -9.355568503977876205, 14.10000000000000142 ) ) ;
#6173 = ORIENTED_EDGE ( 'NONE', *, *, #1838, .T. ) ;
#6174 = CARTESIAN_POINT ( 'NONE',  ( 11.31370849898482334, -11.31370849898469366, 45.00000000000000711 ) ) ;
#6175 = CARTESIAN_POINT ( 'NONE',  ( 7.771249796623105333, 7.842167650704653603, 4.748862081921425116 ) ) ;
#6176 = CARTESIAN_POINT ( 'NONE',  ( 8.512513224245308763, 13.54758718765259040, 7.285714285714284699 ) ) ;
#6177 = CONTEXT_DEPENDENT_SHAPE_REPRESENTATION ( #7655, #4265 ) ;
#6178 = CARTESIAN_POINT ( 'NONE',  ( 11.85413878919593422, 7.448449071214774619, 25.71428571428571885 ) ) ;
#6179 = CARTESIAN_POINT ( 'NONE',  ( 4.503970704919991519, -13.25633410266674517, 37.43261199819787066 ) ) ;
#6180 = CARTESIAN_POINT ( 'NONE',  ( -4.534861676072319270, 8.900167166472117586, 6.149999999999979927 ) ) ;
#6181 = VERTEX_POINT ( 'NONE', #10037 ) ;
#6182 = CARTESIAN_POINT ( 'NONE',  ( -4.619798703721853528, -13.59724543428036725, 48.06738800180213644 ) ) ;
#6183 = ORIENTED_EDGE ( 'NONE', *, *, #7014, .F. ) ;
#6184 = PLANE ( 'NONE',  #1277 ) ;
#6185 = CARTESIAN_POINT ( 'NONE',  ( 13.96533075980324234, -8.621071003556521006, 16.78167371608784819 ) ) ;
#6186 = CARTESIAN_POINT ( 'NONE',  ( -8.731428362939187338, 13.89598863503036164, 6.214285714285717077 ) ) ;
#6187 = CARTESIAN_POINT ( 'NONE',  ( 1.533232399700100945, -9.375578539472073203, 11.79886208192143471 ) ) ;
#6188 = ADVANCED_FACE ( 'NONE', ( #5489 ), #694, .T. ) ;
#6189 = CARTESIAN_POINT ( 'NONE',  ( 8.841785722321695573, -13.82664651025757152, 29.21024514465927879 ) ) ;
#6190 = CARTESIAN_POINT ( 'NONE',  ( 10.37072757624895836, -1.642561882922355831, 1.200000000000034373 ) ) ;
#6191 = CARTESIAN_POINT ( 'NONE',  ( 9.377220287599001836, 4.724406229267489543, 14.90113791807857879 ) ) ;
#6192 = CARTESIAN_POINT ( 'NONE',  ( 8.084771497730057628E-16, -16.99999999999997868, 2.081899558550498307E-15 ) ) ;
#6193 = ADVANCED_FACE ( 'NONE', ( #8646 ), #10091, .T. ) ;
#6194 = CARTESIAN_POINT ( 'NONE',  ( -4.503970704919988854, 13.25633410266674517, 40.43261199819787066 ) ) ;
#6195 = EDGE_CURVE ( 'NONE', #9252, #3550, #9374, .T. ) ;
#6196 = CARTESIAN_POINT ( 'NONE',  ( 1.441234910513245149, 13.92619789766829008, 8.853102287516419366 ) ) ;
#6197 = CARTESIAN_POINT ( 'NONE',  ( 10.37072757624895836, -1.642561882922355609, 7.199999999999984190 ) ) ;
#6198 = CARTESIAN_POINT ( 'NONE',  ( 15.89939535829187278, 1.791431617653015174, 32.14285714285714590 ) ) ;
#6199 = DIRECTION ( 'NONE',  ( 0.000000000000000000, -6.338944243255235518E-49, 1.000000000000000000 ) ) ;
#6200 = CARTESIAN_POINT ( 'NONE',  ( -7.340858601237953529, -11.92174236212700222, 30.28167371608785530 ) ) ;
#6201 = CARTESIAN_POINT ( 'NONE',  ( 10.36326688006723984, -1.689666864740210883, 9.201137918078538647 ) ) ;
#6202 = CARTESIAN_POINT ( 'NONE',  ( -4.490180821391513533, 8.922933199037158758, 5.151137918078567246 ) ) ;
#6203 = FACE_OUTER_BOUND ( 'NONE', #7664, .T. ) ;
#6204 = CARTESIAN_POINT ( 'NONE',  ( -13.61519076058348254, -8.404922754268771001, 44.71832628391215536 ) ) ;
#6205 = CARTESIAN_POINT ( 'NONE',  ( -4.503970704919988854, 13.25633410266674517, 10.43261199819786356 ) ) ;
#6206 = CARTESIAN_POINT ( 'NONE',  ( -10.15407889436378852, -10.15407889436390576, 46.50000000000002132 ) ) ;
#6207 = ORIENTED_EDGE ( 'NONE', *, *, #6034, .T. ) ;
#6208 = CARTESIAN_POINT ( 'NONE',  ( 5.297344310588354865, 15.53355953199867301, 15.06738800180213822 ) ) ;
#6209 = CARTESIAN_POINT ( 'NONE',  ( -165.0000000000000284, -1.734723475976807094E-15, 3.000000000000002665 ) ) ;
#6210 = CARTESIAN_POINT ( 'NONE',  ( -8.731428362939189114, 13.89598863503036341, 42.21428571428572241 ) ) ;
#6211 = DIRECTION ( 'NONE',  ( 1.000000000000000000, 0.000000000000000000, 0.000000000000000000 ) ) ;
#6212 = DIRECTION ( 'NONE',  ( 1.000000000000000000, 4.755747939841215952E-17, -0.000000000000000000 ) ) ;
#6213 = CARTESIAN_POINT ( 'NONE',  ( 9.865911304835474738, 1.562606840307950051, 13.04999999999999538 ) ) ;
#6214 = CARTESIAN_POINT ( 'NONE',  ( 1.562606840307832368, 9.865911304835510265, 0.4499999999999856337 ) ) ;
#6215 = ADVANCED_FACE ( 'NONE', ( #5535, #4764 ), #2287, .F. ) ;
#6216 = DIRECTION ( 'NONE',  ( -1.000000000000000000, -0.000000000000000000, -0.000000000000000000 ) ) ;
#6217 = CARTESIAN_POINT ( 'NONE',  ( 1.791431617652837316, 15.89939535829188877, 36.85714285714286120 ) ) ;
#6218 = SURFACE_STYLE_FILL_AREA ( #3074 ) ;
#6219 = CARTESIAN_POINT ( 'NONE',  ( 1.917699372585825790, 15.88516839912900203, 22.86118342676929061 ) ) ;
#6220 = CARTESIAN_POINT ( 'NONE',  ( 11.31370849898482334, -11.31370849898469366, 15.00000000000000000 ) ) ;
#6221 = DIRECTION ( 'NONE',  ( -1.000000000000000000, -1.387778780781445676E-16, -0.000000000000000000 ) ) ;
#6222 = EDGE_LOOP ( 'NONE', ( #3796, #2421, #5819, #8936 ) ) ;
#6223 = CARTESIAN_POINT ( 'NONE',  ( -1.837501619626328297, 16.30827793483733856, 0.6428571428571432378 ) ) ;
#6224 = CARTESIAN_POINT ( 'NONE',  ( 5.420364854932000931, 15.49051278174644075, 43.07142857142857650 ) ) ;
#6225 = ADVANCED_FACE ( 'NONE', ( #3731, #9425 ), #8591, .F. ) ;
#6226 = CARTESIAN_POINT ( 'NONE',  ( 1.677562661911645714, 10.91227292449346642, 13.44886208192141197 ) ) ;
#6227 = CARTESIAN_POINT ( 'NONE',  ( 5.420364854932001819, 15.49051278174644430, 1.071428571428570287 ) ) ;
#6228 = EDGE_CURVE ( 'NONE', #8149, #5107, #9473, .T. ) ;
#6229 = CARTESIAN_POINT ( 'NONE',  ( -13.55419868402807992, -4.742819248065651472, 34.92857142857143771 ) ) ;
#6230 = CARTESIAN_POINT ( 'NONE',  ( -4.312909747525649706, -8.464561979789499091, 11.09999999999999787 ) ) ;
#6231 = CARTESIAN_POINT ( 'NONE',  ( -9.355568503977838901, -4.766900247265279944, 17.39999999999997016 ) ) ;
#6232 = CARTESIAN_POINT ( 'NONE',  ( 7.340858601237956194, 11.92174236212700045, 39.28167371608785174 ) ) ;
#6233 = CARTESIAN_POINT ( 'NONE',  ( 15.89939535829187278, 1.791431617653015174, 2.142857142857140573 ) ) ;
#6234 = DIRECTION ( 'NONE',  ( -4.755747939841215952E-17, 1.000000000000000000, 0.000000000000000000 ) ) ;
#6235 = CARTESIAN_POINT ( 'NONE',  ( -15.44746603149413922, -5.543385399275820191, 18.92453085894499409 ) ) ;
#6236 = CARTESIAN_POINT ( 'NONE',  ( -8.512513224245306986, -13.54758718765259218, 10.28571428571428648 ) ) ;
#6237 = CARTESIAN_POINT ( 'NONE',  ( 8.922933199037192509, -4.490180821391404287, 8.348862081921442524 ) ) ;
#6238 = CARTESIAN_POINT ( 'NONE',  ( 1.967016585148662289, -16.29368510291087091, 29.63881657323071295 ) ) ;
#6239 = CARTESIAN_POINT ( 'NONE',  ( -7.071067811865514585, 7.071067811865452413, 0.000000000000000000 ) ) ;
#6240 = CARTESIAN_POINT ( 'NONE',  ( -1.642561882922479732, 10.37072757624896191, 9.299999999999975842 ) ) ;
#6241 = DIRECTION ( 'NONE',  ( 1.000000000000000000, -0.000000000000000000, -0.000000000000000000 ) ) ;
#6242 =( NAMED_UNIT ( * ) SI_UNIT ( $, .STERADIAN. ) SOLID_ANGLE_UNIT ( ) );
#6243 = VERTEX_POINT ( 'NONE', #8012 ) ;
#6244 = CARTESIAN_POINT ( 'NONE',  ( 4.619798703721856192, 13.59724543428036725, 3.067388001802140884 ) ) ;
#6245 = APPLICATION_CONTEXT ( 'automotive_design' ) ;
#6246 = CARTESIAN_POINT ( 'NONE',  ( 7.806708723663832394, 7.806708723663930982, 0.7499999999999762412 ) ) ;
#6247 = CARTESIAN_POINT ( 'NONE',  ( 13.54758718765249803, 8.512513224245457977, 13.71428571428571352 ) ) ;
#6248 = ADVANCED_FACE ( 'NONE', ( #8853 ), #3365, .T. ) ;
#6249 = CARTESIAN_POINT ( 'NONE',  ( -6.182472321793581601E-16, 13.00000000000000178, 0.000000000000000000 ) ) ;
#6250 = CARTESIAN_POINT ( 'NONE',  ( -7.390897758835869524, 7.458344646081637386, 2.001137918078543354 ) ) ;
#6251 = CARTESIAN_POINT ( 'NONE',  ( 4.490180821391514421, -8.922933199037132113, 6.651137918078563693 ) ) ;
#6252 = CARTESIAN_POINT ( 'NONE',  ( -163.1342507503006232, -1.077664609596973300, 12.95579008069663551 ) ) ;
#6253 = CARTESIAN_POINT ( 'NONE',  ( 11.92174236212692229, 7.340858601238088532, 5.718326283912152697 ) ) ;
#6254 = CARTESIAN_POINT ( 'NONE',  ( 13.17239914596754424, -4.743843029824685864, 0.5754691410550027975 ) ) ;
#6255 = EDGE_LOOP ( 'NONE', ( #302, #9622, #8000, #4673 ) ) ;
#6256 = CARTESIAN_POINT ( 'NONE',  ( 13.96533075980324234, -8.621071003556521006, 4.781673716087850856 ) ) ;
#6257 = DIRECTION ( 'NONE',  ( -0.7071067811865350272, 8.659560562355083235E-17, -0.7071067811865598962 ) ) ;
#6258 = CARTESIAN_POINT ( 'NONE',  ( -8.512513224245306986, -13.54758718765259218, 46.28571428571429180 ) ) ;
#6259 = DIRECTION ( 'NONE',  ( -5.102127870520027391E-17, 1.000000000000000000, 0.000000000000000000 ) ) ;
#6260 = CARTESIAN_POINT ( 'NONE',  ( -6.717514421272238856, 6.717514421272180236, 15.00000000000001421 ) ) ;
#6261 = CARTESIAN_POINT ( 'NONE',  ( 8.900167166472154889, -4.534861676072210912, 1.350000000000015188 ) ) ;
#6262 = DIRECTION ( 'NONE',  ( -1.000000000000000000, -0.000000000000000000, -0.000000000000000000 ) ) ;
#6263 = CARTESIAN_POINT ( 'NONE',  ( -1.917699372585823570, -15.88516839912900558, 31.86118342676929416 ) ) ;
#6264 = CARTESIAN_POINT ( 'NONE',  ( 1.707986654103998303, -16.32287076676380266, 37.64689771248358596 ) ) ;
#6265 = VECTOR ( 'NONE', #8185, 1000.000000000000000 ) ;
#6266 = AXIS2_PLACEMENT_3D ( 'NONE', #4682, #6998, #10111 ) ;
#6267 = AXIS2_PLACEMENT_3D ( 'NONE', #8699, #1768, #9637 ) ;
#6268 = CARTESIAN_POINT ( 'NONE',  ( 1.791431617652837316, 15.89939535829188877, 12.85714285714285943 ) ) ;
#6269 = LINE ( 'NONE', #9453, #3140 ) ;
#6270 = VERTEX_POINT ( 'NONE', #9730 ) ;
#6271 = CARTESIAN_POINT ( 'NONE',  ( 16.30827793483735633, -1.837501619626142890, 2.357142857142856762 ) ) ;
#6272 =( LENGTH_UNIT ( ) NAMED_UNIT ( * ) SI_UNIT ( .MILLI., .METRE. ) );
#6273 = MECHANICAL_DESIGN_GEOMETRIC_PRESENTATION_REPRESENTATION (  '', ( #9437 ), #4476 ) ;
#6274 = STYLED_ITEM ( 'NONE', ( #3490 ), #206 ) ;
#6275 = VECTOR ( 'NONE', #5481, 1000.000000000000000 ) ;
#6276 = CARTESIAN_POINT ( 'NONE',  ( 10.89658364409024749, 1.776620879821585897, 8.048862081921450695 ) ) ;
#6277 = CARTESIAN_POINT ( 'NONE',  ( 11.60466159355862104, 11.60466159355875071, 7.500000000000005329 ) ) ;
#6278 = CARTESIAN_POINT ( 'NONE',  ( 8.731428362939190890, -13.89598863503036164, 15.21428571428571530 ) ) ;
#6279 = CARTESIAN_POINT ( 'NONE',  ( -10.15407889436378852, -10.15407889436390398, 34.50000000000000000 ) ) ;
#6280 = CARTESIAN_POINT ( 'NONE',  ( -4.312909747525649706, -8.464561979789507973, 5.099999999999993427 ) ) ;
#6281 = CARTESIAN_POINT ( 'NONE',  ( -7.458344646081709328, 7.390897758835804687, 0.9988620819214170110 ) ) ;
#6282 = EDGE_LOOP ( 'NONE', ( #7580, #2344, #2721, #4461 ) ) ;
#6283 = CARTESIAN_POINT ( 'NONE',  ( 9.899494936611718643, -9.899494936611608509, 9.000000000000001776 ) ) ;
#6284 = ORIENTED_EDGE ( 'NONE', *, *, #4186, .T. ) ;
#6285 = CARTESIAN_POINT ( 'NONE',  ( 4.000000000000003553, 0.000000000000000000, 0.000000000000000000 ) ) ;
#6286 = CARTESIAN_POINT ( 'NONE',  ( -16.32287076676382398, 1.707986654103809343, 31.35310228751642470 ) ) ;
#6287 = CARTESIAN_POINT ( 'NONE',  ( 1.837501619626329630, -16.30827793483733501, 9.642857142857144126 ) ) ;
#6288 = CARTESIAN_POINT ( 'NONE',  ( 5.404401153735178376, -15.06016580658422477, 23.42453085894499409 ) ) ;
#6289 = DIRECTION ( 'NONE',  ( 0.2882273949230682586, -0.9575619921529162637, -1.755378125195845577E-33 ) ) ;
#6291 = AXIS2_PLACEMENT_3D ( 'NONE', #3652, #6789, #10117 ) ;
#6290 = CARTESIAN_POINT ( 'NONE',  ( -1.727091770866549414, -10.90442828429184274, 7.950000000000040146 ) ) ;
#6292 = DIRECTION ( 'NONE',  ( -1.000000000000000000, 0.000000000000000000, 0.000000000000000000 ) ) ;
#6293 = AXIS2_PLACEMENT_3D ( 'NONE', #3144, #9469, #6337 ) ;
#6294 = SURFACE_STYLE_FILL_AREA ( #3308 ) ;
#6295 = VERTEX_POINT ( 'NONE', #4916 ) ;
#6296 = CARTESIAN_POINT ( 'NONE',  ( 7.750357176954296712, -12.08964793087877787, 17.21024514465927879 ) ) ;
#6297 = CARTESIAN_POINT ( 'NONE',  ( 10.37072757624895836, -1.642561882922355609, 10.19999999999998685 ) ) ;
#6298 = CARTESIAN_POINT ( 'NONE',  ( -15.89939535829186923, -1.791431617653016062, 11.14285714285714235 ) ) ;
#6299 = CARTESIAN_POINT ( 'NONE',  ( -88.00000000000002842, 0.000000000000000000, 0.000000000000000000 ) ) ;
#6300 = CARTESIAN_POINT ( 'NONE',  ( -7.750357176954294935, 12.08964793087877787, 32.21024514465928235 ) ) ;
#6301 = CARTESIAN_POINT ( 'NONE',  ( -1.595456901104623348, 10.37818827243067155, 5.301137918078554279 ) ) ;
#6302 = CARTESIAN_POINT ( 'NONE',  ( -4.967534682030703586, 9.859792900771061852, -0.8488620819214613977 ) ) ;
#6303 = CARTESIAN_POINT ( 'NONE',  ( -68.00000000000002842, 0.000000000000000000, 18.00000000000000355 ) ) ;
#6304 = CARTESIAN_POINT ( 'NONE',  ( -4.865839792409144771, -13.51115193377589740, 2.075469141055009015 ) ) ;
#6305 = AXIS2_PLACEMENT_3D ( 'NONE', #8023, #5740, #9688 ) ;
#6306 = CARTESIAN_POINT ( 'NONE',  ( 9.809645194534072132, -9.989344678689256796, 19.00404056962642940 ) ) ;
#6307 = EDGE_LOOP ( 'NONE', ( #2766, #9048, #6585, #2139 ) ) ;
#6308 = CARTESIAN_POINT ( 'NONE',  ( 15.14410076328353227, -5.164528828830166063, 16.56738800180213289 ) ) ;
#6309 = DIRECTION ( 'NONE',  ( 0.2882273949230689802, 0.9575619921529161527, -1.755378125195851735E-33 ) ) ;
#6310 = CARTESIAN_POINT ( 'NONE',  ( -8.731428362939189114, 13.89598863503036341, 48.21428571428570820 ) ) ;
#6311 = CARTESIAN_POINT ( 'NONE',  ( 8.787954181158717404, -8.913453481710838844, -1.270000000000007123 ) ) ;
#6312 = DIRECTION ( 'NONE',  ( 1.000000000000000000, 0.000000000000000000, 0.000000000000000000 ) ) ;
#6313 = CARTESIAN_POINT ( 'NONE',  ( 8.464561979789474222, 4.312909747525755400, 15.90000000000002522 ) ) ;
#6314 = CARTESIAN_POINT ( 'NONE',  ( -9.383039235653820143, 1.486127417882155521, 8.700000000000041922 ) ) ;
#6315 = CARTESIAN_POINT ( 'NONE',  ( 0.000000000000000000, -1.018491042385001544, 0.000000000000000000 ) ) ;
#6316 = CARTESIAN_POINT ( 'NONE',  ( 1.562606840307832146, 9.865911304835508489, 0.4499999999999857447 ) ) ;
#6317 = CARTESIAN_POINT ( 'NONE',  ( -16.29368510291090288, 1.967016585148476215, 39.36118342676930837 ) ) ;
#6318 = ORIENTED_EDGE ( 'NONE', *, *, #6034, .F. ) ;
#6319 = CARTESIAN_POINT ( 'NONE',  ( -13.89598863503046111, 8.731428362939027465, 17.78571428571428115 ) ) ;
#6320 =( BOUNDED_CURVE ( )  B_SPLINE_CURVE ( 2, ( #3335, #8030, #5653, #6316, #6367, #125, #4885, #960, #1537, #7880, #9545, #859, #5552, #7255, #177, #4733, #1633, #5450, #9392, #4683, #5506, #9449, #7984, #806, #911, #8761, #4779, #3955, #7930, #2452, #5598, #1689, #4831, #3198, #6280, #6132, #4649, #5567, #3088, #1448, #2317, #6180, #9308, #2419, #7803, #4029, #2987, #6333, #725, #4698, #7751, #2221, #771, #10123, #10071, #3918, #7124, #40, #7016, #3973, #9513, #10173, #8728, #1649, #7894, #877, #5367, #4796, #3873, #8523, #3824, #9357, #7949, #4597, #6230, #2267, #9407, #672, #6961, #3040, #5469, #5414, #8572, #8629, #819, #7845, #1496, #1551, #7063, #10226, #3136, #9465, #2367, #5519, #8678, #1600, #4749, #1703, #976, #2572, #7223, #5001, #90, #141, #300, #8147, #8883, #4124, #6435, #1851, #1127, #7273, #8990, #5669, #5762, #8101, #7325, #6383, #7173, #8934, #8785, #199, #4848, #9664, #6581, #9618, #1030, #7373, #4176, #3351, #3442 ),
 .UNSPECIFIED., .F., .T. ) 
 B_SPLINE_CURVE_WITH_KNOTS ( ( 3, 2, 2, 2, 2, 2, 2, 2, 2, 2, 2, 2, 2, 2, 2, 2, 2, 2, 2, 2, 2, 2, 2, 2, 2, 2, 2, 2, 2, 2, 2, 2, 2, 2, 2, 2, 2, 2, 2, 2, 2, 2, 2, 2, 2, 2, 2, 2, 2, 2, 2, 2, 2, 2, 2, 2, 2, 2, 2, 2, 2, 2, 2, 2, 2, 3 ),
 ( 0.000000000000000000, 0.01428571428571428527, 0.02857142857142857054, 0.04285714285714285060, 0.05714285714285714107, 0.07142857142857142461, 0.08571428571428570120, 0.1000000000000000056, 0.1142857142857142821, 0.1285714285714285587, 0.1428571428571428492, 0.1571428571428571397, 0.1714285714285714024, 0.1857142857142857206, 0.2000000000000000111, 0.2142857142857142738, 0.2285714285714285643, 0.2428571428571428548, 0.2571428571428571175, 0.2714285714285714080, 0.2857142857142856984, 0.2999999999999999889, 0.3142857142857142794, 0.3285714285714285698, 0.3428571428571428048, 0.3571428571428571508, 0.3714285714285714413, 0.3857142857142857317, 0.4000000000000000222, 0.4142857142857143127, 0.4285714285714285476, 0.4428571428571428381, 0.4571428571428571286, 0.4714285714285714191, 0.4857142857142857095, 0.5000000000000000000, 0.5142857142857142350, 0.5285714285714285809, 0.5428571428571428159, 0.5571428571428571619, 0.5714285714285713969, 0.5857142857142857428, 0.5999999999999999778, 0.6142857142857143238, 0.6285714285714285587, 0.6428571428571429047, 0.6571428571428571397, 0.6714285714285713746, 0.6857142857142856096, 0.6999999999999999556, 0.7142857142857143016, 0.7285714285714285365, 0.7428571428571428825, 0.7571428571428571175, 0.7714285714285714635, 0.7857142857142856984, 0.8000000000000000444, 0.8142857142857143904, 0.8285714285714286254, 0.8428571428571428603, 0.8571428571428570953, 0.8714285714285714413, 0.8857142857142856762, 0.9000000000000000222, 0.9142857142857142572, 0.9285714285714286031 ),
 .UNSPECIFIED. ) 
 CURVE ( )  GEOMETRIC_REPRESENTATION_ITEM ( )  RATIONAL_B_SPLINE_CURVE ( ( 1.000000000000000000, 0.9510565162951535312, 1.000000000000000000, 0.9510565162951535312, 1.000000000000000000, 0.9510565162951535312, 1.000000000000000000, 0.9510565162951535312, 1.000000000000000000, 0.9510565162951535312, 1.000000000000000000, 0.9510565162951535312, 1.000000000000000000, 0.9510565162951535312, 1.000000000000000000, 0.9510565162951535312, 1.000000000000000000, 0.9510565162951535312, 1.000000000000000000, 0.9510565162951535312, 1.000000000000000000, 0.9510565162951535312, 1.000000000000000000, 0.9510565162951535312, 1.000000000000000000, 0.9510565162951535312, 1.000000000000000000, 0.9510565162951535312, 1.000000000000000000, 0.9510565162951535312, 1.000000000000000000, 0.9510565162951535312, 1.000000000000000000, 0.9510565162951535312, 1.000000000000000000, 0.9510565162951535312, 1.000000000000000000, 0.9510565162951535312, 1.000000000000000000, 0.9510565162951535312, 1.000000000000000000, 0.9510565162951535312, 1.000000000000000000, 0.9510565162951535312, 1.000000000000000000, 0.9510565162951535312, 1.000000000000000000, 0.9510565162951535312, 1.000000000000000000, 0.9510565162951535312, 1.000000000000000000, 0.9510565162951535312, 1.000000000000000000, 0.9510565162951535312, 1.000000000000000000, 0.9510565162951535312, 1.000000000000000000, 0.9510565162951535312, 1.000000000000000000, 0.9510565162951535312, 1.000000000000000000, 0.9510565162951535312, 1.000000000000000000, 0.9510565162951535312, 1.000000000000000000, 0.9510565162951535312, 1.000000000000000000, 0.9510565162951535312, 1.000000000000000000, 0.9510565162951535312, 1.000000000000000000, 0.9510565162951535312, 1.000000000000000000, 0.9510565162951535312, 1.000000000000000000, 0.9510565162951535312, 1.000000000000000000, 0.9510565162951535312, 1.000000000000000000, 0.9510565162951535312, 1.000000000000000000, 0.9510565162951535312, 1.000000000000000000, 0.9510565162951535312, 1.000000000000000000, 0.9510565162951535312, 1.000000000000000000, 0.9510565162951535312, 1.000000000000000000, 0.9510565162951535312, 1.000000000000000000, 0.9510565162951535312, 1.000000000000000000, 0.9510565162951535312, 1.000000000000000000, 0.9510565162951535312, 1.000000000000000000, 0.9510565162951535312, 1.000000000000000000, 0.9510565162951535312, 1.000000000000000000, 0.9510565162951535312, 1.000000000000000000, 0.9510565162951535312, 1.000000000000000000, 0.9510565162951535312, 1.000000000000000000, 0.9510565162951535312, 1.000000000000000000, 0.9510565162951535312, 1.000000000000000000, 0.9510565162951535312, 1.000000000000000000, 0.9510565162951535312, 1.000000000000000000, 0.9510565162951535312, 1.000000000000000000, 0.9510565162951535312, 1.000000000000000000, 0.9510565162951535312, 1.000000000000000000, 0.9510565162951535312, 1.000000000000000000, 0.9510565162951535312, 1.000000000000000000, 0.9510565162951535312, 1.000000000000000000, 0.9510565162951535312, 1.000000000000000000, 0.9510565162951535312, 1.000000000000000000 ) ) 
 REPRESENTATION_ITEM ( '' )  );
#6321 = CARTESIAN_POINT ( 'NONE',  ( 11.09109556827038467, 11.02177121192640818, 48.73000000000001819 ) ) ;
#6322 = EDGE_LOOP ( 'NONE', ( #1772, #5749 ) ) ;
#6323 = CARTESIAN_POINT ( 'NONE',  ( -11.31370849898482156, 11.31370849898469544, 0.000000000000000000 ) ) ;
#6324 = SURFACE_STYLE_USAGE ( .BOTH. , #4739 ) ;
#6325 = CARTESIAN_POINT ( 'NONE',  ( 9.859792900771104485, -4.967534682030585458, 20.34886208192140700 ) ) ;
#6326 = CIRCLE ( 'NONE', #2842, 8.200000000000009948 ) ;
#6327 = CARTESIAN_POINT ( 'NONE',  ( -7.771249796623103556, -7.842167650704634063, 9.248862081921457090 ) ) ;
#6328 = CARTESIAN_POINT ( 'NONE',  ( 15.53355953199861794, 5.297344310588528060, -0.06738800180213055935 ) ) ;
#6329 = CARTESIAN_POINT ( 'NONE',  ( 15.49051278174638036, 5.420364854932175014, 19.92857142857143771 ) ) ;
#6330 = APPLICATION_PROTOCOL_DEFINITION ( 'draft international standard', 'automotive_design', 1998, #10155 ) ;
#6331 = CARTESIAN_POINT ( 'NONE',  ( 7.448449071214646722, 11.85413878919601594, 37.28571428571429180 ) ) ;
#6332 = CARTESIAN_POINT ( 'NONE',  ( -1.478298951650703019, 14.28433602490913579, 34.64689771248358596 ) ) ;
#6333 = CARTESIAN_POINT ( 'NONE',  ( 9.865911304835478290, 1.562606840307950051, 7.050000000000010481 ) ) ;
#6334 = CARTESIAN_POINT ( 'NONE',  ( 9.355568503977840678, 4.766900247265305701, 15.90000000000002522 ) ) ;
#6335 = ORIENTED_EDGE ( 'NONE', *, *, #5565, .T. ) ;
#6336 = CARTESIAN_POINT ( 'NONE',  ( -9.899494936611716867, 9.899494936611610285, 0.000000000000000000 ) ) ;
#6337 = DIRECTION ( 'NONE',  ( 0.7071067811865505703, -0.7071067811865444641, 0.000000000000000000 ) ) ;
#6338 = ADVANCED_FACE ( 'NONE', ( #3994 ), #7238, .T. ) ;
#6339 = CARTESIAN_POINT ( 'NONE',  ( 8.731428362939189114, -13.89598863503035986, 15.21428571428571708 ) ) ;
#6340 = CARTESIAN_POINT ( 'NONE',  ( -11.51250119794888072, -11.69682198916848037, 24.49595943037356705 ) ) ;
#6341 = CARTESIAN_POINT ( 'NONE',  ( -7.806708723663830618, -7.806708723663906113, 2.249999999999986233 ) ) ;
#6342 = CARTESIAN_POINT ( 'NONE',  ( 4.766900247265192903, 9.355568503977902850, 0.5999999999999894307 ) ) ;
#6343 = ADVANCED_FACE ( 'NONE', ( #1666 ), #7140, .T. ) ;
#6344 = DIRECTION ( 'NONE',  ( -1.387778780781445676E-16, 1.000000000000000000, 0.000000000000000000 ) ) ;
#6345 =( NAMED_UNIT ( * ) PLANE_ANGLE_UNIT ( ) SI_UNIT ( $, .RADIAN. ) );
#6346 = CARTESIAN_POINT ( 'NONE',  ( 15.10213328493390783, -5.284464991282587398, 32.57142857142856940 ) ) ;
#6347 = ORIENTED_EDGE ( 'NONE', *, *, #9121, .T. ) ;
#6348 = CARTESIAN_POINT ( 'NONE',  ( -10.06191849875405531, -10.24623928997363542, 18.49595943037356705 ) ) ;
#6349 = CARTESIAN_POINT ( 'NONE',  ( -9.355568503977838901, -4.766900247265279944, 17.39999999999997016 ) ) ;
#6350 = CARTESIAN_POINT ( 'NONE',  ( 15.89939535829187278, 1.791431617653015174, 14.14285714285714413 ) ) ;
#6351 = CARTESIAN_POINT ( 'NONE',  ( -163.4344937688939865, 0.5323397972486557661, 12.98948098652724603 ) ) ;
#6352 = CARTESIAN_POINT ( 'NONE',  ( 7.390897758835871301, -7.458344646081618734, 0.5011379180785839882 ) ) ;
#6353 = CARTESIAN_POINT ( 'NONE',  ( -9.873755945037078874, -1.513077731353019706, 13.55113791807856316 ) ) ;
#6354 = ADVANCED_FACE ( 'NONE', ( #991 ), #6499, .F. ) ;
#6355 = CARTESIAN_POINT ( 'NONE',  ( -108.0000000000000284, 1.959434878635765131E-15, -16.00000000000000000 ) ) ;
#6356 = CARTESIAN_POINT ( 'NONE',  ( 7.529642458189280241, -12.22833218042435099, 7.218326283912148256 ) ) ;
#6357 = CARTESIAN_POINT ( 'NONE',  ( -13.92619789766827054, -1.441234910513399470, 9.146897712483580634 ) ) ;
#6358 = ORIENTED_EDGE ( 'NONE', *, *, #7789, .F. ) ;
#6359 = ADVANCED_FACE ( 'NONE', ( #8951, #9633 ), #1812, .F. ) ;
#6360 = CYLINDRICAL_SURFACE ( 'NONE', #9203, 2.000000000000000888 ) ;
#6361 = CARTESIAN_POINT ( 'NONE',  ( -5.284464991282755264, 15.10213328493384743, 48.42857142857143060 ) ) ;
#6362 = DIRECTION ( 'NONE',  ( 0.000000000000000000, 1.000000000000000000, 0.000000000000000000 ) ) ;
#6363 = CARTESIAN_POINT ( 'NONE',  ( 8.900167166472154889, -4.534861676072210912, 19.34999999999996945 ) ) ;
#6364 = CARTESIAN_POINT ( 'NONE',  ( -6.717514421272238856, 6.717514421272181124, 6.000000000000005329 ) ) ;
#6365 = CARTESIAN_POINT ( 'NONE',  ( 0.000000000000000000, 0.000000000000000000, -1.270000000000007123 ) ) ;
#6366 = CARTESIAN_POINT ( 'NONE',  ( 13.82664651025767100, -8.841785722321541030, 24.78975485534072476 ) ) ;
#6367 = CARTESIAN_POINT ( 'NONE',  ( 4.312909747525650594, 8.464561979789532842, 0.5999999999999894307 ) ) ;
#6368 = CARTESIAN_POINT ( 'NONE',  ( -13.82664651025767100, 8.841785722321537477, 39.78975485534073186 ) ) ;
#6369 = PRESENTATION_LAYER_ASSIGNMENT (  '', '', ( #2590 ) ) ;
#6370 = VERTEX_POINT ( 'NONE', #4968 ) ;
#6371 = CARTESIAN_POINT ( 'NONE',  ( -11.31370849898482156, 11.31370849898469544, 36.00000000000000711 ) ) ;
#6372 = CARTESIAN_POINT ( 'NONE',  ( -7.848420429648667707, 11.63161085820113527, -5.255698201876048165E-17 ) ) ;
#6373 = ORIENTED_EDGE ( 'NONE', *, *, #6893, .T. ) ;
#6374 = CARTESIAN_POINT ( 'NONE',  ( 15.49051278174638036, 5.420364854932175014, 7.928571428571430602 ) ) ;
#6375 = PRESENTATION_STYLE_ASSIGNMENT (( #82 ) ) ;
#6376 = CARTESIAN_POINT ( 'NONE',  ( 4.270415729527831772, 8.486213763410688671, 1.598862081921434308 ) ) ;
#6377 = CARTESIAN_POINT ( 'NONE',  ( 9.333916720356675967, 4.809394265263123636, 13.89886208192141126 ) ) ;
#6378 = CARTESIAN_POINT ( 'NONE',  ( -7.529642458189277576, 12.22833218042435455, 40.21832628391215536 ) ) ;
#6379 = CARTESIAN_POINT ( 'NONE',  ( 5.420364854932001819, 15.49051278174644430, 19.07142857142856940 ) ) ;
#6380 = CARTESIAN_POINT ( 'NONE',  ( 4.623906867372411078, -13.21436662431711717, 39.42857142857143060 ) ) ;
#6381 = CARTESIAN_POINT ( 'NONE',  ( -1.707986654103994528, 16.32287076676380266, -1.353102287516420921 ) ) ;
#6382 = CARTESIAN_POINT ( 'NONE',  ( -10.15407889436378852, -10.15407889436390576, 10.50000000000000533 ) ) ;
#6383 = CARTESIAN_POINT ( 'NONE',  ( -9.865911304835474738, -1.562606840307925626, 17.55000000000002913 ) ) ;
#6384 = CARTESIAN_POINT ( 'NONE',  ( 10.37072757624895836, -1.642561882922355831, 19.19999999999999574 ) ) ;
#6385 = EDGE_LOOP ( 'NONE', ( #9976, #8103 ) ) ;
#6386 = CARTESIAN_POINT ( 'NONE',  ( -12.15899005565164792, 7.639999817571651697, 5.785714285714282035 ) ) ;
#6387 = ORIENTED_EDGE ( 'NONE', *, *, #7867, .T. ) ;
#6388 = CARTESIAN_POINT ( 'NONE',  ( -10.60660171779826833, 10.60660171779815286, 0.000000000000000000 ) ) ;
#6389 =( GEOMETRIC_REPRESENTATION_CONTEXT ( 3 ) GLOBAL_UNCERTAINTY_ASSIGNED_CONTEXT ( ( #3287 ) ) GLOBAL_UNIT_ASSIGNED_CONTEXT ( ( #7007, #6897, #1440 ) ) REPRESENTATION_CONTEXT ( 'NONE', 'WORKASPACE' ) );
#6390 = CARTESIAN_POINT ( 'NONE',  ( 8.512513224245308763, 13.54758718765259040, 19.28571428571428825 ) ) ;
#6391 = CARTESIAN_POINT ( 'NONE',  ( -15.14410076328353227, 5.164528828830164287, 43.56738800180213644 ) ) ;
#6392 = CARTESIAN_POINT ( 'NONE',  ( -10.90442828429183919, -1.727091770866654663, 11.54999999999998295 ) ) ;
#6393 = CARTESIAN_POINT ( 'NONE',  ( -9.837026868206066865, 5.012215536711413399, 8.850000000000008527 ) ) ;
#6394 = DIRECTION ( 'NONE',  ( 6.162975822039154730E-32, 1.332267629550187849E-15, 1.000000000000000000 ) ) ;
#6395 = DIRECTION ( 'NONE',  ( 1.000000000000000000, 1.387778780781445676E-16, 0.000000000000000000 ) ) ;
#6396 = CARTESIAN_POINT ( 'NONE',  ( 13.47998361472151529, 8.620103694222146729, 27.71024514465928235 ) ) ;
#6397 = ORIENTED_EDGE ( 'NONE', *, *, #8994, .T. ) ;
#6398 = CARTESIAN_POINT ( 'NONE',  ( -7.340858601237953529, -11.92174236212700222, 18.28167371608785174 ) ) ;
#6399 = CARTESIAN_POINT ( 'NONE',  ( 7.806708723663832394, 7.806708723663930982, 12.75000000000000355 ) ) ;
#6400 = CARTESIAN_POINT ( 'NONE',  ( -15.49051278174638036, -5.420364854932175902, 10.92857142857142883 ) ) ;
#6401 = DIRECTION ( 'NONE',  ( 0.000000000000000000, 6.938893903907220674E-18, 1.000000000000000000 ) ) ;
#6402 = CARTESIAN_POINT ( 'NONE',  ( -14.28433602490915000, 1.478298951650542481, 43.35310228751642825 ) ) ;
#6403 = CARTESIAN_POINT ( 'NONE',  ( 1.595456901104624459, -10.37818827243064490, 6.801137918078597799 ) ) ;
#6404 = CARTESIAN_POINT ( 'NONE',  ( 9.873755945037075321, 1.513077731353044131, 12.05113791807856671 ) ) ;
#6405 = CARTESIAN_POINT ( 'NONE',  ( -58.00000000000002132, 7.703719777548943412E-30, -1.059261469412979719E-30 ) ) ;
#6406 = CARTESIAN_POINT ( 'NONE',  ( 4.503970704919991519, -13.25633410266674517, 1.432611998197868219 ) ) ;
#6407 = PRESENTATION_STYLE_ASSIGNMENT (( #3372 ) ) ;
#6408 = CARTESIAN_POINT ( 'NONE',  ( -14.25515036105622890, 1.737328882695209575, 9.361183426769292382 ) ) ;
#6409 = ORIENTED_EDGE ( 'NONE', *, *, #585, .T. ) ;
#6410 = CARTESIAN_POINT ( 'NONE',  ( -163.3500000000000512, -1.734723475976807094E-15, 13.00000000000000355 ) ) ;
#6411 = CARTESIAN_POINT ( 'NONE',  ( 5.284464991282756152, -15.10213328493384743, 39.42857142857143060 ) ) ;
#6412 = LINE ( 'NONE', #9589, #6144 ) ;
#6413 = DIRECTION ( 'NONE',  ( 0.000000000000000000, 0.000000000000000000, 1.000000000000000000 ) ) ;
#6414 = CARTESIAN_POINT ( 'NONE',  ( -7.063212654743466601, -7.063212654743531438, 17.25000000000003553 ) ) ;
#6415 = CARTESIAN_POINT ( 'NONE',  ( -9.865911304835474738, -1.562606840307925626, 5.549999999999999822 ) ) ;
#6416 = CYLINDRICAL_SURFACE ( 'NONE', #5119, 17.72919999999999874 ) ;
#6417 = CARTESIAN_POINT ( 'NONE',  ( -5.543385399275643444, -15.44746603149420494, 26.07546914105500235 ) ) ;
#6418 = CARTESIAN_POINT ( 'NONE',  ( 2.000000000000001776, 0.8865213383406900238, 1.535499999999967446 ) ) ;
#6419 = EDGE_CURVE ( 'NONE', #3031, #4139, #7341, .T. ) ;
#6420 = CARTESIAN_POINT ( 'NONE',  ( -15.53355953199861794, -5.297344310588530725, 26.93261199819786356 ) ) ;
#6421 = VERTEX_POINT ( 'NONE', #5683 ) ;
#6422 = STYLED_ITEM ( 'NONE', ( #6770 ), #286 ) ;
#6423 = CARTESIAN_POINT ( 'NONE',  ( -5.284464991282755264, 15.10213328493384743, 36.42857142857143060 ) ) ;
#6424 = CARTESIAN_POINT ( 'NONE',  ( 3.834211569871422309, 14.40628620492435630, -1.793508096673564591E-16 ) ) ;
#6425 = CARTESIAN_POINT ( 'NONE',  ( -8.731428362939189114, 13.89598863503036341, 6.214285714285717965 ) ) ;
#6426 = CYLINDRICAL_SURFACE ( 'NONE', #18, 8.000000000000000000 ) ;
#6427 = CARTESIAN_POINT ( 'NONE',  ( -8.922933199037192509, 4.490180821391424715, 6.848862081921446077 ) ) ;
#6428 = CARTESIAN_POINT ( 'NONE',  ( -1.689666864740335228, 10.36326688006723273, 19.29886208192143471 ) ) ;
#6429 = CARTESIAN_POINT ( 'NONE',  ( -13.17239914596754424, 4.743843029824683200, 45.57546914105501656 ) ) ;
#6430 = AXIS2_PLACEMENT_3D ( 'NONE', #3422, #6560, #5695 ) ;
#6431 = CARTESIAN_POINT ( 'NONE',  ( -8.731428362939189114, 13.89598863503036341, 18.21428571428571885 ) ) ;
#6432 = CARTESIAN_POINT ( 'NONE',  ( -13.21436662431716869, 4.623906867372262752, 41.57142857142856940 ) ) ;
#6433 = CARTESIAN_POINT ( 'NONE',  ( -13.92619789766827054, -1.441234910513399470, 39.14689771248358596 ) ) ;
#6434 = CARTESIAN_POINT ( 'NONE',  ( -7.639999817571787588, 12.15899005565156266, 6.214285714285717965 ) ) ;
#6435 = CARTESIAN_POINT ( 'NONE',  ( 9.383039235653818366, -1.486127417882131097, 16.19999999999999218 ) ) ;
#6436 = CARTESIAN_POINT ( 'NONE',  ( -1.677562661911643938, -10.91227292449344688, 11.94886208192145993 ) ) ;
#6437 = ORIENTED_EDGE ( 'NONE', *, *, #5776, .T. ) ;
#6438 = CARTESIAN_POINT ( 'NONE',  ( -12.22833218042443271, 7.529642458189139909, 49.78167371608785885 ) ) ;
#6439 = AXIS2_PLACEMENT_3D ( 'NONE', #31, #3185, #3812 ) ;
#6440 = EDGE_LOOP ( 'NONE', ( #9358, #3580, #7339, #356 ) ) ;
#6441 = AXIS2_PLACEMENT_3D ( 'NONE', #5353, #2304, #8556 ) ;
#6442 = CARTESIAN_POINT ( 'NONE',  ( 0.000000000000000000, 0.000000000000000000, 113.2548339959390518 ) ) ;
#6443 = AXIS2_PLACEMENT_3D ( 'NONE', #8164, #422, #7392 ) ;
#6444 = CARTESIAN_POINT ( 'NONE',  ( -5.284464991282755264, 15.10213328493384743, 18.42857142857143415 ) ) ;
#6445 = CARTESIAN_POINT ( 'NONE',  ( -15.88516839912898071, -1.917699372586004980, 31.13881657323070939 ) ) ;
#6446 = CARTESIAN_POINT ( 'NONE',  ( 4.766900247265192903, 9.355568503977902850, 12.59999999999999964 ) ) ;
#6447 = CARTESIAN_POINT ( 'NONE',  ( -10.37072757624895836, 1.642561882922381145, 8.700000000000041922 ) ) ;
#6448 = DIRECTION ( 'NONE',  ( 0.000000000000000000, 8.191099868251446680E-34, 1.000000000000000000 ) ) ;
#6449 = CIRCLE ( 'NONE', #189, 1.649999999999984812 ) ;
#6450 = ORIENTED_EDGE ( 'NONE', *, *, #2096, .T. ) ;
#6451 = CARTESIAN_POINT ( 'NONE',  ( -7.750357176954294935, 12.08964793087877787, 20.21024514465928235 ) ) ;
#6452 = CARTESIAN_POINT ( 'NONE',  ( 9.355568503977840678, 4.766900247265305701, 9.900000000000019895 ) ) ;
#6453 = DIRECTION ( 'NONE',  ( -1.000000000000000000, 1.842239752758738928E-31, -1.780435181894459419E-32 ) ) ;
#6454 = CARTESIAN_POINT ( 'NONE',  ( 8.512513224245308763, 13.54758718765259040, 37.28571428571429180 ) ) ;
#6455 = CARTESIAN_POINT ( 'NONE',  ( 10.06191849875406064, 10.24623928997363187, 45.49595943037356705 ) ) ;
#6456 = CARTESIAN_POINT ( 'NONE',  ( -7.842167650704559456, -7.771249796623180828, 13.25113791807857311 ) ) ;
#6457 = CARTESIAN_POINT ( 'NONE',  ( 8.486213763410640709, 4.270415729527937465, 14.90113791807857879 ) ) ;
#6458 = LINE ( 'NONE', #6504, #2638 ) ;
#6459 = CARTESIAN_POINT ( 'NONE',  ( 7.556039541191335474, 11.78653521626503320, 17.28975485534072121 ) ) ;
#6460 = SURFACE_SIDE_STYLE ('',( #6218 ) ) ;
#6461 = CARTESIAN_POINT ( 'NONE',  ( -7.529642458189277576, 12.22833218042435455, 10.21832628391215358 ) ) ;
#6462 = VERTEX_POINT ( 'NONE', #5779 ) ;
#6463 = DIRECTION ( 'NONE',  ( -1.000000000000000000, -0.000000000000000000, -0.000000000000000000 ) ) ;
#6464 = CARTESIAN_POINT ( 'NONE',  ( -11.51250119794888072, -11.69682198916848037, 12.49595943037356349 ) ) ;
#6465 = CARTESIAN_POINT ( 'NONE',  ( -165.8276565213533900, -1.431463064465520851, 12.92108891611541566 ) ) ;
#6466 = CARTESIAN_POINT ( 'NONE',  ( -166.4201884169622758, -1.620235114669962950, 14.91256936275685341 ) ) ;
#6467 = EDGE_CURVE ( 'NONE', #10190, #5950, #1763, .T. ) ;
#6468 = CARTESIAN_POINT ( 'NONE',  ( -8.486213763410637156, -4.270415729527911708, 10.40113791807857524 ) ) ;
#6469 = CARTESIAN_POINT ( 'NONE',  ( -1.562606840307830591, -9.865911304835478290, 10.95000000000000462 ) ) ;
#6470 = CARTESIAN_POINT ( 'NONE',  ( -164.7175697302053834, 2.136007004543084342, 12.82334789677917364 ) ) ;
#6471 = CARTESIAN_POINT ( 'NONE',  ( 13.55419868402807992, 4.742819248065648807, 31.92857142857143415 ) ) ;
#6472 = CARTESIAN_POINT ( 'NONE',  ( -5.164528828830334817, 15.14410076328347543, 28.43261199819786356 ) ) ;
#6473 = EDGE_LOOP ( 'NONE', ( #311, #2177, #1513, #1663 ) ) ;
#6474 = CARTESIAN_POINT ( 'NONE',  ( 15.49051278174638036, 5.420364854932175014, 25.92857142857142705 ) ) ;
#6475 = DIRECTION ( 'NONE',  ( 0.7071067811865510144, -0.7071067811865440200, 0.000000000000000000 ) ) ;
#6476 = CARTESIAN_POINT ( 'NONE',  ( -8.512513224245306986, -13.54758718765259218, 16.28571428571428470 ) ) ;
#6477 = CARTESIAN_POINT ( 'NONE',  ( -1.533232399700100057, 9.375578539472094519, 10.29886208192143293 ) ) ;
#6478 = CARTESIAN_POINT ( 'NONE',  ( -4.724406229267374968, -9.377220287599040915, 15.09886208192144430 ) ) ;
#6479 = UNCERTAINTY_MEASURE_WITH_UNIT (LENGTH_MEASURE( 1.000000000000000082E-05 ), #5379, 'distance_accuracy_value', 'NONE');
#6480 = CARTESIAN_POINT ( 'NONE',  ( 4.865839792409144771, 13.51115193377589740, 47.07546914105501656 ) ) ;
#6481 = CARTESIAN_POINT ( 'NONE',  ( 1.837501619626330074, -16.30827793483733501, 15.64285714285714235 ) ) ;
#6482 = SURFACE_STYLE_FILL_AREA ( #1847 ) ;
#6483 = CARTESIAN_POINT ( 'NONE',  ( -7.529642458189277576, 12.22833218042435455, 40.21832628391215536 ) ) ;
#6484 = PRODUCT_RELATED_PRODUCT_CATEGORY ( 'part', '', ( #1874 ) ) ;
#6485 = CARTESIAN_POINT ( 'NONE',  ( 12.15899005565164792, -7.639999817571655250, 14.78571428571429358 ) ) ;
#6486 = CARTESIAN_POINT ( 'NONE',  ( 8.787954181158717404, -8.913453481710838844, 0.000000000000000000 ) ) ;
#6487 = CARTESIAN_POINT ( 'NONE',  ( -7.458344646081709328, 7.390897758835804687, 9.998862081921425116 ) ) ;
#6488 = ORIENTED_EDGE ( 'NONE', *, *, #1414, .T. ) ;
#6489 = CARTESIAN_POINT ( 'NONE',  ( 10.15407889436379030, 10.15407889436390576, 1.500000000000003553 ) ) ;
#6490 = ORIENTED_EDGE ( 'NONE', *, *, #9471, .T. ) ;
#6491 = CARTESIAN_POINT ( 'NONE',  ( 57.99999999999997158, 9.797174393178825657E-16, -8.000000000000000000 ) ) ;
#6492 = CARTESIAN_POINT ( 'NONE',  ( 16.30827793483735633, -1.837501619626142890, 14.35714285714285587 ) ) ;
#6493 = CARTESIAN_POINT ( 'NONE',  ( -11.51250119794888072, -11.69682198916848037, 36.49595943037355994 ) ) ;
#6494 = CARTESIAN_POINT ( 'NONE',  ( -5.012215536711506658, 9.837026868206027785, 9.150000000000003908 ) ) ;
#6495 = CARTESIAN_POINT ( 'NONE',  ( 10.90442828429183919, 1.727091770866679532, 13.04999999999999538 ) ) ;
#6496 = CARTESIAN_POINT ( 'NONE',  ( -4.742819248065500481, -13.55419868402813499, 4.071428571428569398 ) ) ;
#6497 = CARTESIAN_POINT ( 'NONE',  ( 9.989344678689365153, -9.809645194533958446, 16.99595943037355994 ) ) ;
#6498 = CARTESIAN_POINT ( 'NONE',  ( -9.355568503977838901, -4.766900247265280832, 14.39999999999996838 ) ) ;
#6499 = CYLINDRICAL_SURFACE ( 'NONE', #7489, 8.200000000000009948 ) ;
#6500 = CARTESIAN_POINT ( 'NONE',  ( -9.989344678689363377, 9.809645194533960222, 43.99595943037355994 ) ) ;
#6501 = CARTESIAN_POINT ( 'NONE',  ( 4.809394265263009061, 9.333916720356739916, 14.60113791807856920 ) ) ;
#6502 = CARTESIAN_POINT ( 'NONE',  ( -7.390897758835869524, 7.458344646081644491, 8.001137918078546463 ) ) ;
#6503 = EDGE_CURVE ( 'NONE', #3093, #7090, #4692, .T. ) ;
#6504 = CARTESIAN_POINT ( 'NONE',  ( -8.084771497730057628E-16, 16.99999999999997868, 0.000000000000000000 ) ) ;
#6505 = CARTESIAN_POINT ( 'NONE',  ( 13.59724543428031573, 4.619798703722006294, 23.93261199819786711 ) ) ;
#6506 = CARTESIAN_POINT ( 'NONE',  ( 13.92619789766827587, 1.441234910513398582, 12.14689771248358063 ) ) ;
#6507 = ORIENTED_EDGE ( 'NONE', *, *, #2096, .F. ) ;
#6508 = CARTESIAN_POINT ( 'NONE',  ( -165.0000000000000284, -1.734723475976807094E-15, 2.008579978604527305 ) ) ;
#6509 = CARTESIAN_POINT ( 'NONE',  ( 8.841785722321695573, -13.82664651025757152, 11.21024514465928235 ) ) ;
#6510 = DIRECTION ( 'NONE',  ( -1.000000000000000000, -0.000000000000000000, -0.000000000000000000 ) ) ;
#6511 = CARTESIAN_POINT ( 'NONE',  ( -163.3797075017903353, -1.420136444163668132, 14.93295499430977991 ) ) ;
#6512 = CARTESIAN_POINT ( 'NONE',  ( -7.098671581784199880, -7.027753727702804376, 7.251137918078588207 ) ) ;
#6513 = CARTESIAN_POINT ( 'NONE',  ( -7.063212654743466601, -7.063212654743534991, 2.249999999999986233 ) ) ;
#6514 = CARTESIAN_POINT ( 'NONE',  ( 6.919986107680329290, -12.02850919814119379, 0.000000000000000000 ) ) ;
#6515 = CARTESIAN_POINT ( 'NONE',  ( -15.06016580658428694, 5.404401153735006957, 39.57546914105500946 ) ) ;
#6516 = CARTESIAN_POINT ( 'NONE',  ( -12.15899005565164792, 7.639999817571651697, 23.78571428571429536 ) ) ;
#6517 = CARTESIAN_POINT ( 'NONE',  ( 16.29368510291089223, -1.967016585148476882, 42.36118342676930126 ) ) ;
#6518 = EDGE_LOOP ( 'NONE', ( #3886, #9205, #8618, #2196 ) ) ;
#6519 = CARTESIAN_POINT ( 'NONE',  ( -8.512513224245306986, -13.54758718765259218, 28.28571428571428825 ) ) ;
#6520 = CARTESIAN_POINT ( 'NONE',  ( 3.104357715559908915, 14.35744100736050655, 7.004981435163800088E-16 ) ) ;
#6521 = CARTESIAN_POINT ( 'NONE',  ( -1.791431617652833763, -15.89939535829188877, 15.85714285714286120 ) ) ;
#6522 = EDGE_CURVE ( 'NONE', #6730, #5950, #5088, .T. ) ;
#6523 = CARTESIAN_POINT ( 'NONE',  ( 1.027016091380565710, 17.97067716999126219, 48.73000000000001819 ) ) ;
#6524 = CARTESIAN_POINT ( 'NONE',  ( -4.312909747525649706, -8.464561979789507973, 2.099999999999990763 ) ) ;
#6525 = CARTESIAN_POINT ( 'NONE',  ( -4.724406229267374968, -9.377220287599040915, 18.09886208192144252 ) ) ;
#6526 = CARTESIAN_POINT ( 'NONE',  ( -9.809645194534070356, 9.989344678689256796, 40.00404056962644006 ) ) ;
#6527 = CARTESIAN_POINT ( 'NONE',  ( 13.54758718765249803, 8.512513224245457977, 25.71428571428571885 ) ) ;
#6528 = EDGE_CURVE ( 'NONE', #5925, #8732, #3560, .T. ) ;
#6529 = CARTESIAN_POINT ( 'NONE',  ( -7.639999817571786700, 12.15899005565156266, 48.21428571428571530 ) ) ;
#6530 = CARTESIAN_POINT ( 'NONE',  ( -4.865839792409144771, -13.51115193377589740, 44.07546914105503078 ) ) ;
#6531 = CARTESIAN_POINT ( 'NONE',  ( 1.607813917173038121, -14.26974319298267346, 15.64285714285714235 ) ) ;
#6532 = CARTESIAN_POINT ( 'NONE',  ( -5.110041130070070992, -16.97680807127747826, -1.270000000000007123 ) ) ;
#6533 = CARTESIAN_POINT ( 'NONE',  ( -4.724406229267374968, -9.377220287599040915, 6.098862081921437195 ) ) ;
#6534 = ORIENTED_EDGE ( 'NONE', *, *, #2801, .T. ) ;
#6535 = CARTESIAN_POINT ( 'NONE',  ( -10.15407889436378852, -10.15407889436390576, 22.50000000000000000 ) ) ;
#6536 = VERTEX_POINT ( 'NONE', #2065 ) ;
#6537 = FACE_OUTER_BOUND ( 'NONE', #378, .T. ) ;
#6538 = CARTESIAN_POINT ( 'NONE',  ( -15.49051278174637858, -5.420364854932175014, 16.92857142857143060 ) ) ;
#6539 = EDGE_CURVE ( 'NONE', #9801, #273, #9979, .T. ) ;
#6540 = CARTESIAN_POINT ( 'NONE',  ( -5.404401153735176599, 15.06016580658422477, 38.42453085894499054 ) ) ;
#6541 = CARTESIAN_POINT ( 'NONE',  ( -10.37072757624895836, 1.642561882922381145, 8.700000000000041922 ) ) ;
#6542 = CARTESIAN_POINT ( 'NONE',  ( 7.806708723663831506, 7.806708723663931870, 18.74999999999998934 ) ) ;
#6543 = CARTESIAN_POINT ( 'NONE',  ( 14.26974319298268767, -1.607813917172876472, 14.35714285714285587 ) ) ;
#6544 = CARTESIAN_POINT ( 'NONE',  ( -13.25633410266679313, 4.503970704919840529, 31.56738800180213644 ) ) ;
#6545 = DIRECTION ( 'NONE',  ( 1.000000000000000000, 0.000000000000000000, 0.000000000000000000 ) ) ;
#6546 = CARTESIAN_POINT ( 'NONE',  ( -16.30827793483735988, 1.837501619626141780, 17.35714285714286476 ) ) ;
#6547 = CARTESIAN_POINT ( 'NONE',  ( -164.5666002992762458, 1.606502708168054738, 12.90062083485027777 ) ) ;
#6548 = CARTESIAN_POINT ( 'NONE',  ( -4.619798703721853528, -13.59724543428036725, 36.06738800180213644 ) ) ;
#6549 = CARTESIAN_POINT ( 'NONE',  ( -4.967534682030703586, 9.859792900771061852, 11.15113791807855215 ) ) ;
#6550 = CARTESIAN_POINT ( 'NONE',  ( 10.91227292449344155, 1.677562661911773390, 0.05113791807855379290 ) ) ;
#6551 = CARTESIAN_POINT ( 'NONE',  ( -70.00000000000001421, 1.040949779275250140E-15, -8.500000000000000000 ) ) ;
#6552 = PRODUCT_DEFINITION_SHAPE ( 'NONE', 'NONE',  #6660 ) ;
#6553 = CARTESIAN_POINT ( 'NONE',  ( -1.693770420379220099, -13.89774397934251837, 25.86118342676929416 ) ) ;
#6554 = CARTESIAN_POINT ( 'NONE',  ( 9.837026868206066865, -5.012215536711391195, 10.35000000000002274 ) ) ;
#6555 = ADVANCED_FACE ( 'NONE', ( #2886, #8160 ), #5216, .F. ) ;
#6556 = EDGE_LOOP ( 'NONE', ( #9551, #1386, #1273, #455 ) ) ;
#6557 = DIRECTION ( 'NONE',  ( 0.000000000000000000, 0.000000000000000000, 1.000000000000000000 ) ) ;
#6558 = CARTESIAN_POINT ( 'NONE',  ( 13.47998361472151529, 8.620103694222146729, 3.710245144659281458 ) ) ;
#6559 = FACE_OUTER_BOUND ( 'NONE', #6892, .T. ) ;
#6560 = DIRECTION ( 'NONE',  ( -1.000000000000000000, 1.842239752758738928E-31, -1.780435181894459419E-32 ) ) ;
#6561 = CARTESIAN_POINT ( 'NONE',  ( -6.683790977649319842, 6.751237864895101026, 5.001137918078545574 ) ) ;
#6562 = CARTESIAN_POINT ( 'NONE',  ( -8.464561979789474222, -4.312909747525728754, 11.39999999999996660 ) ) ;
#6563 = FACE_OUTER_BOUND ( 'NONE', #335, .T. ) ;
#6564 = CARTESIAN_POINT ( 'NONE',  ( 13.91197093850538380, 1.567502665446386390, 32.14285714285714590 ) ) ;
#6565 = EDGE_CURVE ( 'NONE', #3127, #10190, #366, .T. ) ;
#6566 = VERTEX_POINT ( 'NONE', #5170 ) ;
#6567 = CARTESIAN_POINT ( 'NONE',  ( -13.89598863503046111, 8.731428362939027465, 29.78571428571428825 ) ) ;
#6568 = CARTESIAN_POINT ( 'NONE',  ( -167.1500000000000341, -6.071532165918824830E-15, 0.000000000000000000 ) ) ;
#6569 = CARTESIAN_POINT ( 'NONE',  ( -15.49051278174638036, -5.420364854932175902, 16.92857142857143771 ) ) ;
#6570 = APPLICATION_CONTEXT ( 'automotive_design' ) ;
#6571 = DIRECTION ( 'NONE',  ( -1.000000000000000000, 1.842239752758738928E-31, -1.780435181894459419E-32 ) ) ;
#6572 = CARTESIAN_POINT ( 'NONE',  ( -8.922933199037192509, 4.490180821391428267, 18.84886208192146029 ) ) ;
#6573 = CARTESIAN_POINT ( 'NONE',  ( -9.858066664633883036, -1.612135949262833323, 3.548862081921419609 ) ) ;
#6574 = UNCERTAINTY_MEASURE_WITH_UNIT (LENGTH_MEASURE( 1.000000000000000082E-05 ), #6809, 'distance_accuracy_value', 'NONE');
#6575 = CARTESIAN_POINT ( 'NONE',  ( -5.543385399275643444, -15.44746603149420494, 8.075469141055007682 ) ) ;
#6576 = CARTESIAN_POINT ( 'NONE',  ( 1.837501619626330074, -16.30827793483733501, 33.64285714285715301 ) ) ;
#6577 = DIRECTION ( 'NONE',  ( 0.000000000000000000, 0.000000000000000000, 1.000000000000000000 ) ) ;
#6578 = CARTESIAN_POINT ( 'NONE',  ( 1.917699372585825790, 15.88516839912900203, 4.861183426769296823 ) ) ;
#6579 = PRESENTATION_LAYER_ASSIGNMENT (  '', '', ( #5298 ) ) ;
#6580 = CARTESIAN_POINT ( 'NONE',  ( -13.21436662431716869, 4.623906867372262752, 11.57142857142857295 ) ) ;
#6581 = CARTESIAN_POINT ( 'NONE',  ( 4.312909747525650594, 8.464561979789532842, 18.60000000000000497 ) ) ;
#6582 = CARTESIAN_POINT ( 'NONE',  ( -10.89658364409024749, -1.776620879821559917, 6.548862081921412504 ) ) ;
#6583 = ORIENTED_EDGE ( 'NONE', *, *, #8348, .F. ) ;
#6584 = CARTESIAN_POINT ( 'NONE',  ( 12.15899005565164792, -7.639999817571655250, 14.78571428571429358 ) ) ;
#6585 = ORIENTED_EDGE ( 'NONE', *, *, #3459, .T. ) ;
#6586 = CARTESIAN_POINT ( 'NONE',  ( 11.31370849898482334, -11.31370849898469366, 33.00000000000000000 ) ) ;
#6587 = AXIS2_PLACEMENT_3D ( 'NONE', #8195, #4074, #4224 ) ;
#6588 = CIRCLE ( 'NONE', #1672, 3.299999999999999822 ) ;
#6589 = CARTESIAN_POINT ( 'NONE',  ( -13.96533075980324234, 8.621071003556515677, 37.78167371608785174 ) ) ;
#6590 = CARTESIAN_POINT ( 'NONE',  ( -7.806708723663830618, -7.806708723663906113, 8.250000000000028422 ) ) ;
#6591 = CARTESIAN_POINT ( 'NONE',  ( 7.639999817571788476, -12.15899005565156266, 15.21428571428571708 ) ) ;
#6592 = AXIS2_PLACEMENT_3D ( 'NONE', #8617, #5509, #7795 ) ;
#6593 = CIRCLE ( 'NONE', #6106, 1.535500000000000087 ) ;
#6594 = AXIS2_PLACEMENT_3D ( 'NONE', #10134, #4609, #2890 ) ;
#6595 = CARTESIAN_POINT ( 'NONE',  ( 10.06191849875406064, 10.24623928997363187, 33.49595943037355994 ) ) ;
#6596 = CARTESIAN_POINT ( 'NONE',  ( 55.99999999999996447, 0.000000000000000000, 0.000000000000000000 ) ) ;
#6597 = DIRECTION ( 'NONE',  ( 1.387778780781445676E-16, -1.000000000000000000, 0.000000000000000000 ) ) ;
#6598 = CARTESIAN_POINT ( 'NONE',  ( -13.51115193377584589, -4.865839792409295761, 36.92453085894499765 ) ) ;
#6599 = CARTESIAN_POINT ( 'NONE',  ( 9.355568503977840678, 4.766900247265305701, 0.9000000000000119016 ) ) ;
#6600 = CARTESIAN_POINT ( 'NONE',  ( 10.91227292449344155, 1.677562661911774944, 9.051137918078573819 ) ) ;
#6601 = PRESENTATION_LAYER_ASSIGNMENT (  '', '', ( #3152 ) ) ;
#6602 = AXIS2_PLACEMENT_3D ( 'NONE', #490, #10050, #4419 ) ;
#6603 = CARTESIAN_POINT ( 'NONE',  ( -9.837026868206066865, 5.012215536711416064, 5.849999999999989875 ) ) ;
#6604 = CARTESIAN_POINT ( 'NONE',  ( -13.96533075980324234, 8.621071003556515677, 37.78167371608785174 ) ) ;
#6605 = CARTESIAN_POINT ( 'NONE',  ( -13.13091431946350163, 7.193069072976622458, 48.73000000000003240 ) ) ;
#6606 = MECHANICAL_DESIGN_GEOMETRIC_PRESENTATION_REPRESENTATION (  '', ( #1690 ), #8051 ) ;
#6607 = CARTESIAN_POINT ( 'NONE',  ( 5.297344310588354865, 15.53355953199867301, 3.067388001802140884 ) ) ;
#6608 = CARTESIAN_POINT ( 'NONE',  ( -55.00000000000002132, 7.703719777548943412E-30, -7.703719777548943412E-31 ) ) ;
#6609 = CARTESIAN_POINT ( 'NONE',  ( -4.355403765523468529, -8.442910196168346815, 7.101137918078564759 ) ) ;
#6610 = CARTESIAN_POINT ( 'NONE',  ( 4.355403765523470305, 8.442910196168369907, -0.3988620819214416247 ) ) ;
#6611 = CARTESIAN_POINT ( 'NONE',  ( -167.1500000000000057, 0.1422526577103273016, 15.00000000000000000 ) ) ;
#6612 = CARTESIAN_POINT ( 'NONE',  ( -1.917699372585823570, -15.88516839912900558, 37.86118342676929416 ) ) ;
#6613 = CARTESIAN_POINT ( 'NONE',  ( 4.623906867372411078, -13.21436662431711717, 27.42857142857143060 ) ) ;
#6614 = CIRCLE ( 'NONE', #8622, 18.00000000000000355 ) ;
#6615 = CARTESIAN_POINT ( 'NONE',  ( -13.55419868402807992, -4.742819248065651472, 40.92857142857145192 ) ) ;
#6616 = ORIENTED_EDGE ( 'NONE', *, *, #9933, .F. ) ;
#6617 = CARTESIAN_POINT ( 'NONE',  ( -15.49051278174638036, -5.420364854932175902, 40.92857142857145192 ) ) ;
#6618 = CARTESIAN_POINT ( 'NONE',  ( 2.511715608995780613, 15.22804288820251806, -2.187087473825319915E-16 ) ) ;
#6619 = CARTESIAN_POINT ( 'NONE',  ( 8.731428362939190890, -13.89598863503036164, 21.21428571428571885 ) ) ;
#6620 = EDGE_CURVE ( 'NONE', #3468, #2524, #2118, .T. ) ;
#6621 = DIRECTION ( 'NONE',  ( 0.2882273949230683141, -0.9575619921529162637, -1.755378125195845919E-33 ) ) ;
#6622 = CARTESIAN_POINT ( 'NONE',  ( 1.513077731352925115, 9.873755945037103743, 19.44886208192144039 ) ) ;
#6623 = CARTESIAN_POINT ( 'NONE',  ( 1.513077731352925115, 9.873755945037098414, 4.448862081921434175 ) ) ;
#6624 = CARTESIAN_POINT ( 'NONE',  ( -1.707986654103994528, 16.32287076676380266, 4.646897712483579745 ) ) ;
#6625 = CARTESIAN_POINT ( 'NONE',  ( -13.54758718765249625, -8.512513224245459753, 28.71428571428571530 ) ) ;
#6626 = DIRECTION ( 'NONE',  ( 0.000000000000000000, 1.000000000000000000, 0.000000000000000000 ) ) ;
#6627 = CARTESIAN_POINT ( 'NONE',  ( -11.69682198916834892, -11.51250119794901394, 8.504040569626438284 ) ) ;
#6628 = AXIS2_PLACEMENT_3D ( 'NONE', #1108, #3377, #2550 ) ;
#6629 = SHAPE_REPRESENTATION ( 'cir_block', ( #3995 ), #8889 ) ;
#6630 = CARTESIAN_POINT ( 'NONE',  ( -1.607813917173034124, 14.26974319298267524, 24.64285714285714235 ) ) ;
#6631 = CARTESIAN_POINT ( 'NONE',  ( -11.31370849898482156, 11.31370849898469544, 5.999999999999998224 ) ) ;
#6632 = CARTESIAN_POINT ( 'NONE',  ( -7.771249796623103556, -7.842167650704634063, 9.248862081921457090 ) ) ;
#6633 = ORIENTED_EDGE ( 'NONE', *, *, #9306, .F. ) ;
#6634 = CARTESIAN_POINT ( 'NONE',  ( -12.15899005565164792, 7.639999817571651697, 11.78571428571428115 ) ) ;
#6635 = VERTEX_POINT ( 'NONE', #9828 ) ;
#6636 = CARTESIAN_POINT ( 'NONE',  ( -15.89939535829186923, -1.791431617653016062, 29.14285714285714235 ) ) ;
#6637 = CARTESIAN_POINT ( 'NONE',  ( -4.743843029824828861, 13.17239914596749450, 2.424530858944988321 ) ) ;
#6638 = CARTESIAN_POINT ( 'NONE',  ( -9.355568503977838901, -4.766900247265279944, 17.39999999999997016 ) ) ;
#6639 = PRODUCT ( 'piston', 'piston', '', ( #9869 ) ) ;
#6640 = CARTESIAN_POINT ( 'NONE',  ( -1.607813917173034124, 14.26974319298267346, 12.64285714285714235 ) ) ;
#6641 = CARTESIAN_POINT ( 'NONE',  ( 13.89774397934249706, 1.693770420379375308, 34.13881657323070584 ) ) ;
#6642 = EDGE_LOOP ( 'NONE', ( #5895, #978, #9726, #354 ) ) ;
#6643 = DIRECTION ( 'NONE',  ( 0.000000000000000000, -6.338944243255235518E-49, 1.000000000000000000 ) ) ;
#6644 = EDGE_CURVE ( 'NONE', #4085, #3486, #1725, .T. ) ;
#6645 = CARTESIAN_POINT ( 'NONE',  ( 9.858066664633883036, 1.612135949262857526, 2.048862081921423162 ) ) ;
#6646 = CARTESIAN_POINT ( 'NONE',  ( 1.567502665446232957, 13.91197093850540156, 0.8571428571428549859 ) ) ;
#6647 = CARTESIAN_POINT ( 'NONE',  ( -4.809394265263009061, -9.333916720356723928, 13.10113791807856920 ) ) ;
#6648 = CARTESIAN_POINT ( 'NONE',  ( 4.967534682030706250, -9.859792900771042312, 3.651137918078570355 ) ) ;
#6649 = CARTESIAN_POINT ( 'NONE',  ( -156.0000000000000284, -6.661338147750945553E-15, 0.000000000000000000 ) ) ;
#6650 =( NAMED_UNIT ( * ) PLANE_ANGLE_UNIT ( ) SI_UNIT ( $, .RADIAN. ) );
#6651 = CARTESIAN_POINT ( 'NONE',  ( -7.556039541191334585, -11.78653521626503320, 20.28975485534072121 ) ) ;
#6652 = CARTESIAN_POINT ( 'NONE',  ( -4.766900247265192014, -9.355568503977876205, 5.099999999999993427 ) ) ;
#6653 = CARTESIAN_POINT ( 'NONE',  ( 1.967016585148662289, -16.29368510291087091, 41.63881657323070584 ) ) ;
#6654 = ORIENTED_EDGE ( 'NONE', *, *, #7313, .T. ) ;
#6655 = CARTESIAN_POINT ( 'NONE',  ( -1.639859883600667700, 13.92277000329989534, 48.73000000000004661 ) ) ;
#6656 = LINE ( 'NONE', #532, #4509 ) ;
#6657 = EDGE_CURVE ( 'NONE', #7090, #6853, #7307, .T. ) ;
#6658 = CARTESIAN_POINT ( 'NONE',  ( 1.612135949262739398, 9.858066664633913234, 2.451137918078564848 ) ) ;
#6659 = CARTESIAN_POINT ( 'NONE',  ( 1.486127417882244783, -9.383039235653791721, 16.80000000000003624 ) ) ;
#6660 = PRODUCT_DEFINITION ( 'UNKNOWN', '', #5417, #4742 ) ;
#6661 = CARTESIAN_POINT ( 'NONE',  ( -164.4418057750100388, 2.081034501115442303, 14.85496774026629119 ) ) ;
#6662 = CARTESIAN_POINT ( 'NONE',  ( -1.607813917173034124, 14.26974319298267524, 24.64285714285714235 ) ) ;
#6663 = CARTESIAN_POINT ( 'NONE',  ( 13.55419868402807992, 4.742819248065648807, 43.92857142857143060 ) ) ;
#6664 = ORIENTED_EDGE ( 'NONE', *, *, #7657, .F. ) ;
#6665 = CARTESIAN_POINT ( 'NONE',  ( -8.731428362939189114, 13.89598863503036341, 42.21428571428572241 ) ) ;
#6666 = DIRECTION ( 'NONE',  ( 0.000000000000000000, 8.191099868251446680E-34, 1.000000000000000000 ) ) ;
#6667 = CARTESIAN_POINT ( 'NONE',  ( -5.420364854931999155, -15.49051278174644253, 16.07142857142857650 ) ) ;
#6668 = CARTESIAN_POINT ( 'NONE',  ( 6.751237864895159646, -6.683790977649233689, 17.49886208192142689 ) ) ;
#6669 = CARTESIAN_POINT ( 'NONE',  ( 9.390499931835536884, -1.439022436064273158, 5.198862081921453715 ) ) ;
#6670 = UNCERTAINTY_MEASURE_WITH_UNIT (LENGTH_MEASURE( 1.000000000000000082E-05 ), #7797, 'distance_accuracy_value', 'NONE');
#6671 = CARTESIAN_POINT ( 'NONE',  ( -13.82664651025767100, 8.841785722321537477, 9.789754855340722983 ) ) ;
#6672 = CARTESIAN_POINT ( 'NONE',  ( -15.49051278174638036, -5.420364854932175902, 28.92857142857143771 ) ) ;
#6673 = CARTESIAN_POINT ( 'NONE',  ( -15.91362231745475597, -1.665163862720028254, 9.146897712483580634 ) ) ;
#6674 = CARTESIAN_POINT ( 'NONE',  ( 13.21436662431716869, -4.623906867372263640, 26.57142857142857295 ) ) ;
#6675 = CARTESIAN_POINT ( 'NONE',  ( 5.420364854932001819, 15.49051278174644430, 1.071428571428570287 ) ) ;
#6676 = CARTESIAN_POINT ( 'NONE',  ( -58.00000000000002842, 5.689893001204698381E-17, 8.200000000000009948 ) ) ;
#6677 = EDGE_LOOP ( 'NONE', ( #42, #2872 ) ) ;
#6678 = CARTESIAN_POINT ( 'NONE',  ( 7.448449071214646722, 11.85413878919601594, 13.28571428571429003 ) ) ;
#6679 = EDGE_CURVE ( 'NONE', #2768, #1705, #1068, .T. ) ;
#6680 = VERTEX_POINT ( 'NONE', #8366 ) ;
#6681 = CARTESIAN_POINT ( 'NONE',  ( -5.284464991282755264, 15.10213328493384743, 36.42857142857143060 ) ) ;
#6682 = CARTESIAN_POINT ( 'NONE',  ( -9.989344678689363377, 9.809645194533960222, 1.995959430373561272 ) ) ;
#6683 = CARTESIAN_POINT ( 'NONE',  ( 9.355568503977840678, 4.766900247265305701, 15.90000000000002522 ) ) ;
#6684 = DIRECTION ( 'NONE',  ( 6.123233995736784525E-17, 2.137782238269831797E-32, -1.000000000000000000 ) ) ;
#6685 = CARTESIAN_POINT ( 'NONE',  ( 9.899494936611718643, -9.899494936611608509, 9.000000000000001776 ) ) ;
#6686 = EDGE_LOOP ( 'NONE', ( #2605, #6728, #2824, #7805, #6450 ) ) ;
#6687 = VECTOR ( 'NONE', #752, 1000.000000000000000 ) ;
#6688 = CARTESIAN_POINT ( 'NONE',  ( 4.619798703721856192, 13.59724543428036725, 21.06738800180213644 ) ) ;
#6689 = ORIENTED_EDGE ( 'NONE', *, *, #7657, .T. ) ;
#6690 = DIRECTION ( 'NONE',  ( 0.000000000000000000, 0.000000000000000000, 1.000000000000000000 ) ) ;
#6691 = CARTESIAN_POINT ( 'NONE',  ( -166.6500000000000341, -1.532656754117495520E-15, 3.000000000000002665 ) ) ;
#6692 = CARTESIAN_POINT ( 'NONE',  ( 9.859792900771104485, -4.967534682030585458, 20.34886208192140700 ) ) ;
#6693 = CARTESIAN_POINT ( 'NONE',  ( 5.012215536711511987, -9.837026868205999364, 4.650000000000026112 ) ) ;
#6694 = CARTESIAN_POINT ( 'NONE',  ( -9.814260835641038128, 5.056896391392219137, 1.851137918078540334 ) ) ;
#6695 = CARTESIAN_POINT ( 'NONE',  ( 9.511495879682431411E-16, -20.00000000000000000, 2.449293598294706513E-15 ) ) ;
#6696 = CARTESIAN_POINT ( 'NONE',  ( -1.693770420379220099, -13.89774397934251837, 31.86118342676929416 ) ) ;
#6697 = DIRECTION ( 'NONE',  ( 4.743101658384303144E-33, -1.040834085586086106E-16, 1.000000000000000000 ) ) ;
#6698 = CARTESIAN_POINT ( 'NONE',  ( 5.012215536711511987, -9.837026868205999364, 4.650000000000026112 ) ) ;
#6699 = CARTESIAN_POINT ( 'NONE',  ( -5.297344310588352201, -15.53355953199867301, 36.06738800180213644 ) ) ;
#6700 = CARTESIAN_POINT ( 'NONE',  ( -3.566842584106372893, 15.58126113556745551, 48.73000000000023135 ) ) ;
#6701 = CARTESIAN_POINT ( 'NONE',  ( -13.54758718765249625, -8.512513224245459753, 22.71428571428571530 ) ) ;
#6702 = DIRECTION ( 'NONE',  ( 0.000000000000000000, -6.338944243255235518E-49, 1.000000000000000000 ) ) ;
#6703 = ADVANCED_FACE ( 'NONE', ( #8320 ), #7595, .T. ) ;
#6704 =( GEOMETRIC_REPRESENTATION_CONTEXT ( 3 ) GLOBAL_UNCERTAINTY_ASSIGNED_CONTEXT ( ( #4943 ) ) GLOBAL_UNIT_ASSIGNED_CONTEXT ( ( #9420, #10136, #8428 ) ) REPRESENTATION_CONTEXT ( 'NONE', 'WORKASPACE' ) );
#6705 = CARTESIAN_POINT ( 'NONE',  ( -1.441234910513241818, -13.92619789766829008, 17.85310228751642114 ) ) ;
#6706 = CARTESIAN_POINT ( 'NONE',  ( -8.486213763410637156, -4.270415729527911708, 13.40113791807857702 ) ) ;
#6707 = CARTESIAN_POINT ( 'NONE',  ( -4.534861676072319270, 8.900167166472121139, 12.14999999999996305 ) ) ;
#6708 = CARTESIAN_POINT ( 'NONE',  ( -68.00000000000002842, 0.000000000000000000, 8.200000000000001066 ) ) ;
#6709 = CARTESIAN_POINT ( 'NONE',  ( -4.623906867372410190, 13.21436662431711895, 48.42857142857143060 ) ) ;
#6710 = CARTESIAN_POINT ( 'NONE',  ( 13.21436662431716869, -4.623906867372263640, 32.57142857142856940 ) ) ;
#6711 = VERTEX_POINT ( 'NONE', #8209 ) ;
#6712 = AXIS2_PLACEMENT_3D ( 'NONE', #2945, #6395, #7136 ) ;
#6713 = CARTESIAN_POINT ( 'NONE',  ( 15.89939535829187278, 1.791431617653015174, 38.14285714285714590 ) ) ;
#6714 = DIRECTION ( 'NONE',  ( 1.000000000000000000, 0.000000000000000000, 0.000000000000000000 ) ) ;
#6715 = CARTESIAN_POINT ( 'NONE',  ( 1.791431617652837316, 15.89939535829188877, 30.85714285714286120 ) ) ;
#6716 = DIRECTION ( 'NONE',  ( -1.000000000000000000, -0.000000000000000000, -0.000000000000000000 ) ) ;
#6717 = PRODUCT_DEFINITION_SHAPE ( 'NONE', 'NONE',  #9288 ) ;
#6718 =( NAMED_UNIT ( * ) SI_UNIT ( $, .STERADIAN. ) SOLID_ANGLE_UNIT ( ) );
#6719 = CARTESIAN_POINT ( 'NONE',  ( -1.513077731352923339, -9.873755945037078874, 14.94886208192145105 ) ) ;
#6720 = CARTESIAN_POINT ( 'NONE',  ( 1.533232399700100945, -9.375578539472067874, 5.798862081921429379 ) ) ;
#6721 = CARTESIAN_POINT ( 'NONE',  ( -1.642561882922479732, 10.37072757624895303, 15.29999999999997939 ) ) ;
#6722 = CARTESIAN_POINT ( 'NONE',  ( -8.620103694221995738, -13.47998361472161299, 8.289754855340721207 ) ) ;
#6723 = CARTESIAN_POINT ( 'NONE',  ( -11.31370849898482156, 11.31370849898469544, 30.00000000000000355 ) ) ;
#6724 = CARTESIAN_POINT ( 'NONE',  ( -13.61519076058348254, -8.404922754268771001, 2.718326283912150476 ) ) ;
#6725 = CARTESIAN_POINT ( 'NONE',  ( 1.607813917173038121, -14.26974319298267346, 21.64285714285714590 ) ) ;
#6726 = CARTESIAN_POINT ( 'NONE',  ( 11.60466159355862104, 11.60466159355875071, 7.500000000000005329 ) ) ;
#6727 = CARTESIAN_POINT ( 'NONE',  ( 5.420364854932001819, 15.49051278174644430, 43.07142857142858361 ) ) ;
#6728 = ORIENTED_EDGE ( 'NONE', *, *, #1185, .F. ) ;
#6729 = CARTESIAN_POINT ( 'NONE',  ( 13.21436662431716869, -4.623906867372263640, 20.57142857142857295 ) ) ;
#6730 = VERTEX_POINT ( 'NONE', #9158 ) ;
#6731 = CARTESIAN_POINT ( 'NONE',  ( -13.54758718765249625, -8.512513224245459753, 28.71428571428571530 ) ) ;
#6732 = CARTESIAN_POINT ( 'NONE',  ( 5.297344310588354865, 15.53355953199867301, 45.06738800180215065 ) ) ;
#6733 = CARTESIAN_POINT ( 'NONE',  ( -4.724406229267374968, -9.377220287599046245, 3.098862081921434974 ) ) ;
#6734 = DIRECTION ( 'NONE',  ( 1.000000000000000000, 0.000000000000000000, 0.000000000000000000 ) ) ;
#6735 = CARTESIAN_POINT ( 'NONE',  ( -4.623906867372410190, 13.21436662431711895, 12.42857142857142705 ) ) ;
#6736 = CARTESIAN_POINT ( 'NONE',  ( 13.25633410266679313, -4.503970704919842305, 22.56738800180214000 ) ) ;
#6737 = VECTOR ( 'NONE', #6289, 1000.000000000000114 ) ;
#6738 = ORIENTED_EDGE ( 'NONE', *, *, #3324, .T. ) ;
#6739 = CARTESIAN_POINT ( 'NONE',  ( 8.672099987835544255, 11.29616555842733661, 48.73000000000003951 ) ) ;
#6740 = CARTESIAN_POINT ( 'NONE',  ( -5.056896391392315948, 9.814260835640997271, 16.14886208192145389 ) ) ;
#6741 = CARTESIAN_POINT ( 'NONE',  ( 14.28433602490915000, -1.478298951650544479, 46.35310228751641404 ) ) ;
#6742 = CARTESIAN_POINT ( 'NONE',  ( 10.90442828429183919, 1.727091770866679310, 7.050000000000010481 ) ) ;
#6743 = CARTESIAN_POINT ( 'NONE',  ( -1.776620879821455556, -10.89658364409025637, 9.951137918078590161 ) ) ;
#6744 = DIRECTION ( 'NONE',  ( 0.000000000000000000, -1.000000000000000000, 0.000000000000000000 ) ) ;
#6745 = CARTESIAN_POINT ( 'NONE',  ( -9.809645194534070356, 9.989344678689256796, 34.00404056962644006 ) ) ;
#6746 = VECTOR ( 'NONE', #1984, 1000.000000000000000 ) ;
#6747 = CIRCLE ( 'NONE', #6932, 0.9906000000000003691 ) ;
#6748 = CIRCLE ( 'NONE', #8254, 17.72919999999999874 ) ;
#6749 = EDGE_LOOP ( 'NONE', ( #9641, #2558, #5988, #6765 ) ) ;
#6750 = CARTESIAN_POINT ( 'NONE',  ( -10.37072757624895836, 1.642561882922381145, 8.700000000000041922 ) ) ;
#6751 = CARTESIAN_POINT ( 'NONE',  ( -15.14410076328353227, 5.164528828830164287, 37.56738800180213644 ) ) ;
#6752 = CARTESIAN_POINT ( 'NONE',  ( -11.48558320758131401, 8.816166900624141434, 48.73000000000002530 ) ) ;
#6753 = CARTESIAN_POINT ( 'NONE',  ( 1.837501619626330074, -16.30827793483733501, 21.64285714285714590 ) ) ;
#6754 = CARTESIAN_POINT ( 'NONE',  ( -170.0000000000000284, -15.00000000000001066, 1.836970198721029983E-15 ) ) ;
#6755 = PRESENTATION_LAYER_ASSIGNMENT (  '', '', ( #2332 ) ) ;
#6756 = AXIS2_PLACEMENT_3D ( 'NONE', #6032, #9212, #9367 ) ;
#6757 = CARTESIAN_POINT ( 'NONE',  ( -11.78653521626494793, -7.556039541191465148, 18.71024514465927879 ) ) ;
#6758 = CARTESIAN_POINT ( 'NONE',  ( -4.490180821391513533, 8.922933199037158758, 17.15113791807853616 ) ) ;
#6759 = CARTESIAN_POINT ( 'NONE',  ( 9.383039235653818366, -1.486127417882130208, 19.19999999999999574 ) ) ;
#6760 = CARTESIAN_POINT ( 'NONE',  ( -167.1500000000000341, -1.102909754258692077E-14, 15.00000000000000000 ) ) ;
#6761 = CARTESIAN_POINT ( 'NONE',  ( 1.917699372585825790, 15.88516839912900203, 40.86118342676929416 ) ) ;
#6762 = CARTESIAN_POINT ( 'NONE',  ( 1.693770420379222319, 13.89774397934251837, -1.138816573230706286 ) ) ;
#6763 = PRESENTATION_LAYER_ASSIGNMENT (  '', '', ( #3653 ) ) ;
#6764 = CARTESIAN_POINT ( 'NONE',  ( 13.55419868402807992, 4.742819248065648807, 31.92857142857143415 ) ) ;
#6765 = ORIENTED_EDGE ( 'NONE', *, *, #6539, .F. ) ;
#6766 = CARTESIAN_POINT ( 'NONE',  ( -16.30827793483735988, 1.837501619626141780, 41.35714285714286120 ) ) ;
#6767 = DIRECTION ( 'NONE',  ( -1.000000000000000000, 0.000000000000000000, 0.000000000000000000 ) ) ;
#6768 = CARTESIAN_POINT ( 'NONE',  ( -15.10213328493390961, 5.284464991282586510, 23.57142857142857650 ) ) ;
#6769 = DIRECTION ( 'NONE',  ( 0.000000000000000000, 0.000000000000000000, 1.000000000000000000 ) ) ;
#6770 = PRESENTATION_STYLE_ASSIGNMENT (( #1260 ) ) ;
#6771 = CARTESIAN_POINT ( 'NONE',  ( -10.90442828429183919, -1.727091770866654663, 2.550000000000035350 ) ) ;
#6772 = CIRCLE ( 'NONE', #3167, 1.535500000000000087 ) ;
#6773 = CARTESIAN_POINT ( 'NONE',  ( -9.383039235653820143, 1.486127417882155299, 2.700000000000035705 ) ) ;
#6774 = CARTESIAN_POINT ( 'NONE',  ( -7.027753727702738651, -7.098671581784262941, 9.248862081921457090 ) ) ;
#6775 = EDGE_CURVE ( 'NONE', #7651, #1651, #9053, .T. ) ;
#6776 = PRODUCT_DEFINITION_CONTEXT ( 'detailed design', #257, 'design' ) ;
#6777 = CARTESIAN_POINT ( 'NONE',  ( 5.012215536711511987, -9.837026868205999364, 10.65000000000000924 ) ) ;
#6778 = AXIS2_PLACEMENT_3D ( 'NONE', #4853, #7280, #2525 ) ;
#6779 = CARTESIAN_POINT ( 'NONE',  ( -13.61519076058348254, -8.404922754268771001, 20.71832628391214826 ) ) ;
#6780 = CARTESIAN_POINT ( 'NONE',  ( 15.10213328493390783, -5.284464991282587398, 44.57142857142857650 ) ) ;
#6781 = FILL_AREA_STYLE_COLOUR ( '', #860 ) ;
#6782 = CARTESIAN_POINT ( 'NONE',  ( 13.82664651025767100, -8.841785722321541030, 18.78975485534072121 ) ) ;
#6783 = CARTESIAN_POINT ( 'NONE',  ( -11.85413878919593422, -7.448449071214776396, 28.71428571428571530 ) ) ;
#6784 = PRODUCT_DEFINITION_SHAPE ( 'NONE', 'NONE',  #10234 ) ;
#6785 = CARTESIAN_POINT ( 'NONE',  ( -13.54758718765249625, -8.512513224245459753, 10.71428571428571708 ) ) ;
#6786 = CARTESIAN_POINT ( 'NONE',  ( -15.89939535829186923, -1.791431617653016062, 47.14285714285714590 ) ) ;
#6787 = ORIENTED_EDGE ( 'NONE', *, *, #2903, .F. ) ;
#6788 = CARTESIAN_POINT ( 'NONE',  ( -10.37072757624895836, 1.642561882922380034, 14.69999999999999041 ) ) ;
#6789 = DIRECTION ( 'NONE',  ( -0.000000000000000000, -0.000000000000000000, -1.000000000000000000 ) ) ;
#6790 = DIRECTION ( 'NONE',  ( 1.000000000000000000, 4.755747939841215952E-17, -0.000000000000000000 ) ) ;
#6791 = EDGE_CURVE ( 'NONE', #7040, #7847, #6326, .T. ) ;
#6792 = CARTESIAN_POINT ( 'NONE',  ( 13.96533075980324234, -8.621071003556521006, 46.78167371608785885 ) ) ;
#6793 = CARTESIAN_POINT ( 'NONE',  ( -7.424621202458789426, 7.424621202458724589, 18.00000000000001421 ) ) ;
#6794 = CARTESIAN_POINT ( 'NONE',  ( -1.791431617652833763, -15.89939535829188877, 3.857142857142857650 ) ) ;
#6795 = SHAPE_DEFINITION_REPRESENTATION ( #2037, #4550 ) ;
#6796 = AXIS2_PLACEMENT_3D ( 'NONE', #2336, #4664, #7033 ) ;
#6797 = CARTESIAN_POINT ( 'NONE',  ( -7.448449071214644945, -11.85413878919601771, 28.28571428571428825 ) ) ;
#6798 = CARTESIAN_POINT ( 'NONE',  ( -1.737328882695368115, 14.25515036105620581, 44.63881657323071295 ) ) ;
#6799 = ORIENTED_EDGE ( 'NONE', *, *, #1838, .F. ) ;
#6800 = DIRECTION ( 'NONE',  ( -0.7071067811865501263, 0.7071067811865450192, 0.000000000000000000 ) ) ;
#6801 = CARTESIAN_POINT ( 'NONE',  ( 15.14410076328353227, -5.164528828830166063, 4.567388001802134667 ) ) ;
#6802 = DIRECTION ( 'NONE',  ( -1.000000000000000000, -1.387778780781445676E-16, 0.000000000000000000 ) ) ;
#6803 = CARTESIAN_POINT ( 'NONE',  ( -1.689666864740335228, 10.36326688006723273, 19.29886208192143471 ) ) ;
#6804 = CARTESIAN_POINT ( 'NONE',  ( -4.623906867372410190, 13.21436662431711895, 0.4285714285714309346 ) ) ;
#6805 = CARTESIAN_POINT ( 'NONE',  ( -5.012215536711506658, 9.837026868206027785, 9.150000000000003908 ) ) ;
#6806 = CARTESIAN_POINT ( 'NONE',  ( -9.377220287598998283, -4.724406229267462898, 10.40113791807857524 ) ) ;
#6807 = DIRECTION ( 'NONE',  ( 0.000000000000000000, -6.338944243255235518E-49, 1.000000000000000000 ) ) ;
#6808 = CARTESIAN_POINT ( 'NONE',  ( -10.24623928997352351, -10.06191849875416899, 32.50404056962644006 ) ) ;
#6809 =( LENGTH_UNIT ( ) NAMED_UNIT ( * ) SI_UNIT ( .MILLI., .METRE. ) );
#6810 = CARTESIAN_POINT ( 'NONE',  ( 9.333916720356675967, 4.809394265263123636, 1.898862081921442790 ) ) ;
#6811 = CARTESIAN_POINT ( 'NONE',  ( 11.40355824106246985, -11.22385875690704538, 40.99595943037355994 ) ) ;
#6812 = CARTESIAN_POINT ( 'NONE',  ( -13.19966323802950114, 7.266400725181457965, 48.73000000000003240 ) ) ;
#6813 = CARTESIAN_POINT ( 'NONE',  ( -1.791431617652833763, -15.89939535829188877, 27.85714285714285765 ) ) ;
#6814 = CARTESIAN_POINT ( 'NONE',  ( -163.9101340986164246, -1.243481348857424562, 12.94061705906631055 ) ) ;
#6815 = EDGE_CURVE ( 'NONE', #2212, #5655, #8637, .T. ) ;
#6816 = AXIS2_PLACEMENT_3D ( 'NONE', #1914, #5979, #5062 ) ;
#6817 = CARTESIAN_POINT ( 'NONE',  ( 13.51115193377584589, 4.865839792409294873, 21.92453085894500120 ) ) ;
#6818 = CARTESIAN_POINT ( 'NONE',  ( -8.486213763410637156, -4.270415729527911708, 16.40113791807857524 ) ) ;
#6819 = CARTESIAN_POINT ( 'NONE',  ( -1.439022436064386845, 9.390499931835535108, 5.301137918078554279 ) ) ;
#6820 = CARTESIAN_POINT ( 'NONE',  ( -167.1360136226436452, -0.2828357332780486177, 12.99766529850317021 ) ) ;
#6821 = CARTESIAN_POINT ( 'NONE',  ( -7.448449071214644945, -11.85413878919601771, 46.28571428571429180 ) ) ;
#6822 = CARTESIAN_POINT ( 'NONE',  ( -9.809645194534070356, 9.989344678689256796, 4.004040569626432067 ) ) ;
#6823 = EDGE_LOOP ( 'NONE', ( #7693, #647 ) ) ;
#6824 = CARTESIAN_POINT ( 'NONE',  ( 1.837501619626330074, -16.30827793483733501, 45.64285714285716011 ) ) ;
#6825 = CARTESIAN_POINT ( 'NONE',  ( 5.986002070941135678, -13.58603705635637304, -1.270000000000007123 ) ) ;
#6826 = CARTESIAN_POINT ( 'NONE',  ( -5.284464991282755264, 15.10213328493384743, 24.42857142857143060 ) ) ;
#6827 = DIRECTION ( 'NONE',  ( -6.162975822039153635E-32, -0.5000000000000011102, -0.8660254037844379305 ) ) ;
#6828 = CARTESIAN_POINT ( 'NONE',  ( 10.90442828429183919, 1.727091770866679532, 1.049999999999966738 ) ) ;
#6829 = CARTESIAN_POINT ( 'NONE',  ( 6.717514421272239744, -6.717514421272154479, 10.50000000000000888 ) ) ;
#6830 = CARTESIAN_POINT ( 'NONE',  ( 8.442910196168311288, 4.355403765523574222, 19.89886208192141481 ) ) ;
#6831 = CARTESIAN_POINT ( 'NONE',  ( 9.355568503977840678, 4.766900247265305701, 12.90000000000002345 ) ) ;
#6832 = CARTESIAN_POINT ( 'NONE',  ( -11.69682198916834892, -11.51250119794901394, 20.50404056962644006 ) ) ;
#6833 = CARTESIAN_POINT ( 'NONE',  ( -1.837501619626328297, 16.30827793483733856, 36.64285714285714590 ) ) ;
#6834 = CARTESIAN_POINT ( 'NONE',  ( -11.69682198916834892, -11.51250119794901394, 26.50404056962643651 ) ) ;
#6835 = CARTESIAN_POINT ( 'NONE',  ( -7.639999817571787588, 12.15899005565156266, 18.21428571428571885 ) ) ;
#6836 = EDGE_CURVE ( 'NONE', #9817, #5655, #574, .T. ) ;
#6837 = DIRECTION ( 'NONE',  ( -0.5000000000000061062, 7.093700570841092585E-34, 0.8660254037844351549 ) ) ;
#6838 = CARTESIAN_POINT ( 'NONE',  ( 8.512513224245308763, 13.54758718765259040, 49.28571428571428470 ) ) ;
#6839 = EDGE_LOOP ( 'NONE', ( #517, #3989, #6738, #4226 ) ) ;
#6840 = CARTESIAN_POINT ( 'NONE',  ( 9.837026868206066865, -5.012215536711392083, 19.34999999999996945 ) ) ;
#6841 = DIRECTION ( 'NONE',  ( 0.000000000000000000, 8.191099868251448390E-34, 1.000000000000000000 ) ) ;
#6842 = CARTESIAN_POINT ( 'NONE',  ( -83.00000000000001421, 0.000000000000000000, 0.000000000000000000 ) ) ;
#6843 = EDGE_CURVE ( 'NONE', #285, #4710, #8636, .T. ) ;
#6844 = CARTESIAN_POINT ( 'NONE',  ( -15.88516839912898071, -1.917699372586004980, 49.13881657323070584 ) ) ;
#6845 = CARTESIAN_POINT ( 'NONE',  ( 1.642561882922480621, -10.37072757624892638, 16.80000000000003624 ) ) ;
#6846 = CARTESIAN_POINT ( 'NONE',  ( -1.837501619626328297, 16.30827793483733856, 0.6428571428571432378 ) ) ;
#6847 = CARTESIAN_POINT ( 'NONE',  ( 13.89598863503046111, -8.731428362939032795, 8.785714285714293581 ) ) ;
#6848 = SHAPE_DEFINITION_REPRESENTATION ( #8218, #6629 ) ;
#6849 = CARTESIAN_POINT ( 'NONE',  ( -13.55419868402807992, -4.742819248065651472, 28.92857142857143415 ) ) ;
#6850 = CARTESIAN_POINT ( 'NONE',  ( 14.25515036105622535, -1.737328882695210241, 24.36118342676929416 ) ) ;
#6851 = VERTEX_POINT ( 'NONE', #9258 ) ;
#6852 = CARTESIAN_POINT ( 'NONE',  ( -4.619798703721853528, -13.59724543428036725, 42.06738800180214355 ) ) ;
#6853 = VERTEX_POINT ( 'NONE', #4556 ) ;
#6854 = FACE_OUTER_BOUND ( 'NONE', #9039, .T. ) ;
#6855 = CARTESIAN_POINT ( 'NONE',  ( -13.47998361472151174, -8.620103694222146729, 18.71024514465927879 ) ) ;
#6856 = CARTESIAN_POINT ( 'NONE',  ( -1.791431617652833763, -15.89939535829188877, 3.857142857142857650 ) ) ;
#6857 = CARTESIAN_POINT ( 'NONE',  ( -9.859792900771106261, 4.967534682030607662, 15.84886208192146739 ) ) ;
#6858 = CARTESIAN_POINT ( 'NONE',  ( 10.37072757624895836, -1.642561882922355831, 1.200000000000034373 ) ) ;
#6859 = CARTESIAN_POINT ( 'NONE',  ( 7.842167650704563897, 7.771249796623202144, 17.75113791807856245 ) ) ;
#6860 = DIRECTION ( 'NONE',  ( 1.000000000000000000, 0.000000000000000000, 0.000000000000000000 ) ) ;
#6861 = CARTESIAN_POINT ( 'NONE',  ( -7.556039541191334585, -11.78653521626503320, 26.28975485534072831 ) ) ;
#6862 = CARTESIAN_POINT ( 'NONE',  ( 10.90442828429183919, 1.727091770866679532, 16.04999999999995808 ) ) ;
#6863 = CARTESIAN_POINT ( 'NONE',  ( -7.750357176954294935, 12.08964793087877787, 2.210245144659280569 ) ) ;
#6864 = CARTESIAN_POINT ( 'NONE',  ( -9.837026868206070418, 5.012215536711412511, 2.849999999999968114 ) ) ;
#6865 = CARTESIAN_POINT ( 'NONE',  ( 15.49051278174638036, 5.420364854932175014, 25.92857142857142705 ) ) ;
#6866 = CARTESIAN_POINT ( 'NONE',  ( 2.000000000000001776, 1.880445160090761061E-16, -1.535500000000000087 ) ) ;
#6867 = AXIS2_PLACEMENT_3D ( 'NONE', #7919, #7300, #9642 ) ;
#6868 = CARTESIAN_POINT ( 'NONE',  ( -10.06191849875405531, -10.24623928997363542, 12.49595943037356349 ) ) ;
#6869 = CARTESIAN_POINT ( 'NONE',  ( -7.390897758835869524, 7.458344646081644491, -0.9988620819214586444 ) ) ;
#6870 = CARTESIAN_POINT ( 'NONE',  ( 7.098671581784200768, 7.027753727702831021, 8.751137918078539357 ) ) ;
#6871 = CARTESIAN_POINT ( 'NONE',  ( 2.000000000000001776, -1.773042676681352292, -1.110223024625156540E-13 ) ) ;
#6872 = CARTESIAN_POINT ( 'NONE',  ( 5.164528828830335705, -15.14410076328347543, 43.43261199819787066 ) ) ;
#6873 = CARTESIAN_POINT ( 'NONE',  ( 1.607813917173038121, -14.26974319298267346, 45.64285714285716011 ) ) ;
#6874 = CARTESIAN_POINT ( 'NONE',  ( 4.865839792409144771, 13.51115193377589740, -0.9245308589449906522 ) ) ;
#6875 = VERTEX_POINT ( 'NONE', #10078 ) ;
#6876 = CARTESIAN_POINT ( 'NONE',  ( -11.51250119794888072, -11.69682198916848037, 6.495959430373559051 ) ) ;
#6877 = DIRECTION ( 'NONE',  ( 0.000000000000000000, 6.338944243255235518E-49, -1.000000000000000000 ) ) ;
#6878 = CARTESIAN_POINT ( 'NONE',  ( 16.30827793483735633, -1.837501619626142890, 26.35714285714285765 ) ) ;
#6879 = MECHANICAL_DESIGN_GEOMETRIC_PRESENTATION_REPRESENTATION (  '', ( #4253 ), #6389 ) ;
#6880 = DIRECTION ( 'NONE',  ( -1.000000000000000000, -0.000000000000000000, -0.000000000000000000 ) ) ;
#6881 =( LENGTH_UNIT ( ) NAMED_UNIT ( * ) SI_UNIT ( .MILLI., .METRE. ) );
#6882 = CARTESIAN_POINT ( 'NONE',  ( 1.642561882922480621, -10.37072757624892638, 1.800000000000023803 ) ) ;
#6883 = CARTESIAN_POINT ( 'NONE',  ( -4.312909747525649706, -8.464561979789499091, 11.09999999999999787 ) ) ;
#6884 = CARTESIAN_POINT ( 'NONE',  ( 4.579542530753127672, -8.877401133907071085, 14.64886208192141659 ) ) ;
#6885 = CARTESIAN_POINT ( 'NONE',  ( -5.986002070941133901, -13.58603705635637304, -1.270000000000007123 ) ) ;
#6886 = CARTESIAN_POINT ( 'NONE',  ( -8.512513224245306986, -13.54758718765259218, 46.28571428571429180 ) ) ;
#6887 = PRODUCT_DEFINITION_FORMATION_WITH_SPECIFIED_SOURCE ( 'ANY', '', #7484, .NOT_KNOWN. ) ;
#6888 = CARTESIAN_POINT ( 'NONE',  ( 1.707986654103998303, -16.32287076676380266, 19.64689771248358596 ) ) ;
#6889 = EDGE_LOOP ( 'NONE', ( #1784, #8631, #2921, #8730 ) ) ;
#6890 = CARTESIAN_POINT ( 'NONE',  ( -8.512513224245306986, -13.54758718765259218, 22.28571428571428470 ) ) ;
#6891 = CARTESIAN_POINT ( 'NONE',  ( -1.837501619626328297, 16.30827793483733856, 48.64285714285716011 ) ) ;
#6892 = EDGE_LOOP ( 'NONE', ( #3538, #5871, #5344, #5601 ) ) ;
#6893 = EDGE_CURVE ( 'NONE', #6181, #7160, #3498, .T. ) ;
#6894 = CARTESIAN_POINT ( 'NONE',  ( 1.642561882922480621, -10.37072757624892638, 13.80000000000003446 ) ) ;
#6895 = SURFACE_STYLE_USAGE ( .BOTH. , #3761 ) ;
#6896 = CARTESIAN_POINT ( 'NONE',  ( -16.30827793483735988, 1.837501619626141558, 41.35714285714286120 ) ) ;
#6897 =( NAMED_UNIT ( * ) PLANE_ANGLE_UNIT ( ) SI_UNIT ( $, .RADIAN. ) );
#6898 = CARTESIAN_POINT ( 'NONE',  ( -9.859792900771106261, 4.967534682030611215, 9.848862081921437195 ) ) ;
#6899 = CARTESIAN_POINT ( 'NONE',  ( 8.731428362939190890, -13.89598863503036164, 9.214285714285717077 ) ) ;
#6900 = CARTESIAN_POINT ( 'NONE',  ( 8.731428362939190890, -13.89598863503036164, 3.214285714285716633 ) ) ;
#6901 = APPLICATION_PROTOCOL_DEFINITION ( 'draft international standard', 'automotive_design', 1998, #9444 ) ;
#6902 = CARTESIAN_POINT ( 'NONE',  ( 13.91197093850538380, 1.567502665446386390, 26.14285714285714590 ) ) ;
#6903 = CARTESIAN_POINT ( 'NONE',  ( -9.809645194534070356, 9.989344678689256796, 34.00404056962644006 ) ) ;
#6904 = CARTESIAN_POINT ( 'NONE',  ( 13.89774397934249706, 1.693770420379375308, 40.13881657323070584 ) ) ;
#6905 = ORIENTED_EDGE ( 'NONE', *, *, #6005, .F. ) ;
#6906 = DIRECTION ( 'NONE',  ( 1.000000000000000000, 0.000000000000000000, 0.000000000000000000 ) ) ;
#6907 = CARTESIAN_POINT ( 'NONE',  ( 11.40355824106246985, -11.22385875690704538, 16.99595943037355994 ) ) ;
#6908 = CARTESIAN_POINT ( 'NONE',  ( -8.512513224245306986, -13.54758718765259218, 4.285714285714288252 ) ) ;
#6909 = CARTESIAN_POINT ( 'NONE',  ( -8.442910196168309511, -4.355403765523544024, 12.39886208192140948 ) ) ;
#6910 = CARTESIAN_POINT ( 'NONE',  ( 1.665163862719847732, 15.91362231745477374, 26.85310228751642470 ) ) ;
#6911 = CARTESIAN_POINT ( 'NONE',  ( -7.424621202458789426, 7.424621202458724589, 6.000000000000005329 ) ) ;
#6912 = CARTESIAN_POINT ( 'NONE',  ( -4.809394265263009061, -9.333916720356723928, 13.10113791807856920 ) ) ;
#6913 = CARTESIAN_POINT ( 'NONE',  ( 16.00000000000000000, 1.959434878635765131E-15, 20.00000000000001776 ) ) ;
#6914 = CARTESIAN_POINT ( 'NONE',  ( -11.92174236212692051, -7.340858601238089420, 32.71832628391215536 ) ) ;
#6915 =( NAMED_UNIT ( * ) PLANE_ANGLE_UNIT ( ) SI_UNIT ( $, .RADIAN. ) );
#6916 = CARTESIAN_POINT ( 'NONE',  ( -13.25633410266679313, 4.503970704919840529, 7.567388001802139108 ) ) ;
#6917 = CARTESIAN_POINT ( 'NONE',  ( -7.806708723663831506, -7.806708723663907001, 2.249999999999986677 ) ) ;
#6918 = CARTESIAN_POINT ( 'NONE',  ( -8.731428362939189114, 13.89598863503036341, 30.21428571428572596 ) ) ;
#6919 = CARTESIAN_POINT ( 'NONE',  ( 14.00000000000000533, 0.000000000000000000, 0.000000000000000000 ) ) ;
#6920 = CARTESIAN_POINT ( 'NONE',  ( 10.06191849875406064, 10.24623928997363187, 21.49595943037356705 ) ) ;
#6921 = CARTESIAN_POINT ( 'NONE',  ( 7.098671581784200768, 7.027753727702823916, 14.75113791807856956 ) ) ;
#6923 = VECTOR ( 'NONE', #3277, 1000.000000000000000 ) ;
#6922 = CARTESIAN_POINT ( 'NONE',  ( -6.683790977649319842, 6.751237864895094809, 2.001137918078543354 ) ) ;
#6924 = VECTOR ( 'NONE', #899, 1000.000000000000000 ) ;
#6925 = CARTESIAN_POINT ( 'NONE',  ( 2.000000000000001776, 1.773042676681366281, 0.000000000000000000 ) ) ;
#6926 = CARTESIAN_POINT ( 'NONE',  ( -8.621071003556675549, 13.96533075980314642, 46.21832628391216247 ) ) ;
#6927 = CARTESIAN_POINT ( 'NONE',  ( 13.91197093850538380, 1.567502665446386390, 38.14285714285714590 ) ) ;
#6928 = CARTESIAN_POINT ( 'NONE',  ( 7.639999817571789364, -12.15899005565156266, 45.21428571428572951 ) ) ;
#6929 = EDGE_LOOP ( 'NONE', ( #6068, #8870 ) ) ;
#6930 = AXIS2_PLACEMENT_3D ( 'NONE', #4326, #9087, #4784 ) ;
#6931 = CARTESIAN_POINT ( 'NONE',  ( -11.51250119794888072, -11.69682198916848037, 12.49595943037356349 ) ) ;
#6932 = AXIS2_PLACEMENT_3D ( 'NONE', #6885, #7788, #10158 ) ;
#6933 = CARTESIAN_POINT ( 'NONE',  ( -108.0000000000000284, 0.000000000000000000, 18.00000000000000355 ) ) ;
#6934 = AXIS2_PLACEMENT_3D ( 'NONE', #2475, #4135, #6448 ) ;
#6935 = CARTESIAN_POINT ( 'NONE',  ( -15.10213328493390961, 5.284464991282586510, 29.57142857142857650 ) ) ;
#6936 = CARTESIAN_POINT ( 'NONE',  ( 2.000000000000001776, 1.773042676681366281, 0.000000000000000000 ) ) ;
#6937 = CARTESIAN_POINT ( 'NONE',  ( 0.2000000000000057288, 0.000000000000000000, 0.000000000000000000 ) ) ;
#6938 = CARTESIAN_POINT ( 'NONE',  ( 4.000000000000003553, 3.500000000000003109, 0.000000000000000000 ) ) ;
#6939 = CARTESIAN_POINT ( 'NONE',  ( -8.464561979789474222, -4.312909747525729642, 8.399999999999963052 ) ) ;
#6940 = CARTESIAN_POINT ( 'NONE',  ( -9.390499931835536884, 1.439022436064298249, 12.69886208192145816 ) ) ;
#6941 = CARTESIAN_POINT ( 'NONE',  ( 5.110041130070070992, -16.97680807127747826, -1.270000000000007123 ) ) ;
#6942 = CARTESIAN_POINT ( 'NONE',  ( 15.06016580658428694, -5.404401153735007846, 18.57546914105500235 ) ) ;
#6943 = CARTESIAN_POINT ( 'NONE',  ( -8.731428362939189114, 13.89598863503036341, 48.21428571428570820 ) ) ;
#6944 = AXIS2_PLACEMENT_3D ( 'NONE', #10204, #1478, #3068 ) ;
#6945 =( GEOMETRIC_REPRESENTATION_CONTEXT ( 3 ) GLOBAL_UNCERTAINTY_ASSIGNED_CONTEXT ( ( #1642 ) ) GLOBAL_UNIT_ASSIGNED_CONTEXT ( ( #1433, #9343, #2045 ) ) REPRESENTATION_CONTEXT ( 'NONE', 'WORKASPACE' ) );
#6946 = SURFACE_STYLE_FILL_AREA ( #605 ) ;
#6947 = CARTESIAN_POINT ( 'NONE',  ( -1.917699372585823570, -15.88516839912900558, 19.86118342676929416 ) ) ;
#6948 = CARTESIAN_POINT ( 'NONE',  ( 15.10213328493390783, -5.284464991282587398, 20.57142857142857295 ) ) ;
#6949 = CARTESIAN_POINT ( 'NONE',  ( 7.833366173951416656, 13.80014417467472398, 48.72999999999998977 ) ) ;
#6950 = EDGE_CURVE ( 'NONE', #5716, #8307, #3643, .T. ) ;
#6951 = CARTESIAN_POINT ( 'NONE',  ( -10.90442828429183919, -1.727091770866654663, 14.55000000000000249 ) ) ;
#6952 = DIRECTION ( 'NONE',  ( 1.000000000000000000, 0.000000000000000000, 0.000000000000000000 ) ) ;
#6953 = CARTESIAN_POINT ( 'NONE',  ( -8.512513224245306986, -13.54758718765259218, 46.28571428571429180 ) ) ;
#6954 = EDGE_CURVE ( 'NONE', #2841, #1237, #9350, .T. ) ;
#6955 = CARTESIAN_POINT ( 'NONE',  ( -5.056896391392315948, 9.814260835640997271, 7.148862081921437017 ) ) ;
#6956 = CARTESIAN_POINT ( 'NONE',  ( -13.89598863503046111, 8.731428362939027465, 5.785714285714282035 ) ) ;
#6957 = CARTESIAN_POINT ( 'NONE',  ( -1.837501619626328297, 16.30827793483733856, 6.642857142857143238 ) ) ;
#6958 = APPLICATION_PROTOCOL_DEFINITION ( 'draft international standard', 'automotive_design', 1998, #7122 ) ;
#6959 = CARTESIAN_POINT ( 'NONE',  ( 4.742819248065502258, 13.55419868402813499, 25.07142857142857650 ) ) ;
#6960 = CARTESIAN_POINT ( 'NONE',  ( -4.865839792409144771, -13.51115193377589740, 38.07546914105502367 ) ) ;
#6961 = CARTESIAN_POINT ( 'NONE',  ( -9.383039235653820143, 1.486127417882154411, 11.69999999999998863 ) ) ;
#6962 = EDGE_LOOP ( 'NONE', ( #5577, #6664, #9777, #4811 ) ) ;
#6963 = CARTESIAN_POINT ( 'NONE',  ( 7.750357176954296712, -12.08964793087877787, 47.21024514465928235 ) ) ;
#6964 = ORIENTED_EDGE ( 'NONE', *, *, #2541, .F. ) ;
#6965 = PLANE ( 'NONE',  #4911 ) ;
#6966 = CARTESIAN_POINT ( 'NONE',  ( 1.967016585148662289, -16.29368510291087091, 23.63881657323070939 ) ) ;
#6967 = CARTESIAN_POINT ( 'NONE',  ( 5.420364854932000931, 15.49051278174644075, 7.071428571428569398 ) ) ;
#6968 = CARTESIAN_POINT ( 'NONE',  ( -7.027753727702738651, -7.098671581784262941, 12.24886208192144998 ) ) ;
#6969 = CARTESIAN_POINT ( 'NONE',  ( 8.404922754268618235, 13.61519076058357491, 27.28167371608785174 ) ) ;
#6970 = CARTESIAN_POINT ( 'NONE',  ( -158.0000000000000284, 17.99999999999999645, 2.204364238465235822E-15 ) ) ;
#6971 = CARTESIAN_POINT ( 'NONE',  ( -10.91227292449344155, -1.677562661911749187, 10.55113791807857204 ) ) ;
#6972 = DIRECTION ( 'NONE',  ( 1.000000000000000000, 0.000000000000000000, 0.000000000000000000 ) ) ;
#6973 = CARTESIAN_POINT ( 'NONE',  ( 13.59724543428031573, 4.619798703722006294, 41.93261199819787066 ) ) ;
#6974 = AXIS2_PLACEMENT_3D ( 'NONE', #8968, #1881, #4153 ) ;
#6975 = CARTESIAN_POINT ( 'NONE',  ( 7.340858601237956194, 11.92174236212700045, 3.281673716087854409 ) ) ;
#6976 = APPLICATION_CONTEXT ( 'automotive_design' ) ;
#6977 = ADVANCED_FACE ( 'NONE', ( #2106, #1330 ), #2925, .F. ) ;
#6978 = CARTESIAN_POINT ( 'NONE',  ( 7.424621202458790314, -7.424621202458697944, 4.500000000000003553 ) ) ;
#6979 = CARTESIAN_POINT ( 'NONE',  ( 16.30827793483735633, -1.837501619626142890, 26.35714285714285765 ) ) ;
#6980 = CARTESIAN_POINT ( 'NONE',  ( -167.1500000000000341, -1.102909754258692077E-14, 15.00000000000000000 ) ) ;
#6981 = CARTESIAN_POINT ( 'NONE',  ( -9.814260835641038128, 5.056896391392221801, 4.851137918078532785 ) ) ;
#6982 = CARTESIAN_POINT ( 'NONE',  ( 1.612135949262739398, 9.858066664633913234, 2.451137918078564848 ) ) ;
#6983 = CARTESIAN_POINT ( 'NONE',  ( -58.00000000000002132, 2.079464148194913600E-15, -18.00000000000000355 ) ) ;
#6984 = CARTESIAN_POINT ( 'NONE',  ( 13.61519076058348254, 8.404922754268771001, 41.71832628391215536 ) ) ;
#6985 = CARTESIAN_POINT ( 'NONE',  ( -12.08964793087886314, 7.750357176954159932, 9.789754855340722983 ) ) ;
#6986 = CARTESIAN_POINT ( 'NONE',  ( -12.15899005565164792, 7.639999817571651697, 47.78571428571430602 ) ) ;
#6987 = VERTEX_POINT ( 'NONE', #3709 ) ;
#6988 = CARTESIAN_POINT ( 'NONE',  ( -5.404401153735176599, 15.06016580658422477, 14.42453085894499232 ) ) ;
#6989 = EDGE_CURVE ( 'NONE', #9103, #6462, #8434, .T. ) ;
#6990 = FACE_OUTER_BOUND ( 'NONE', #7137, .T. ) ;
#6991 = CARTESIAN_POINT ( 'NONE',  ( 11.60466159355862104, 11.60466159355875071, 43.50000000000000711 ) ) ;
#6992 = CIRCLE ( 'NONE', #2380, 1.000000000000000888 ) ;
#6993 = DIRECTION ( 'NONE',  ( -1.000000000000000000, 4.575525868300071581E-16, 0.000000000000000000 ) ) ;
#6994 = CARTESIAN_POINT ( 'NONE',  ( -58.00000000000002132, 8.200000000000009948, 5.769589564291770364E-16 ) ) ;
#6995 = EDGE_CURVE ( 'NONE', #9252, #1309, #2174, .T. ) ;
#6996 = CARTESIAN_POINT ( 'NONE',  ( 7.063212654743467489, 7.063212654743559860, 3.749999999999997335 ) ) ;
#6997 = CARTESIAN_POINT ( 'NONE',  ( -8.922933199037192509, 4.490180821391428267, 18.84886208192146029 ) ) ;
#6998 = DIRECTION ( 'NONE',  ( 1.000000000000000000, 4.755747939841215952E-17, -0.000000000000000000 ) ) ;
#6999 = CARTESIAN_POINT ( 'NONE',  ( -15.49051278174638036, -5.420364854932175902, 40.92857142857145192 ) ) ;
#7000 = FILL_AREA_STYLE_COLOUR ( '', #1021 ) ;
#7001 = CARTESIAN_POINT ( 'NONE',  ( 5.164528828830335705, -15.14410076328347543, 19.43261199819785645 ) ) ;
#7002 = CARTESIAN_POINT ( 'NONE',  ( -1.837501619626328297, 16.30827793483733856, 18.64285714285715656 ) ) ;
#7003 = CARTESIAN_POINT ( 'NONE',  ( 6.421061802350969572, 14.56668498259507949, 48.73000000000001108 ) ) ;
#7004 = CARTESIAN_POINT ( 'NONE',  ( -4.766900247265192014, -9.355568503977876205, 17.10000000000000497 ) ) ;
#7005 = DIRECTION ( 'NONE',  ( 0.000000000000000000, 1.000000000000000000, -1.332267629550187849E-15 ) ) ;
#7006 = CARTESIAN_POINT ( 'NONE',  ( 13.54758718765249803, 8.512513224245457977, 43.71428571428572241 ) ) ;
#7007 =( LENGTH_UNIT ( ) NAMED_UNIT ( * ) SI_UNIT ( .MILLI., .METRE. ) );
#7008 = MANIFOLD_SOLID_BREP ( 'Body', #4159 ) ;
#7009 = CARTESIAN_POINT ( 'NONE',  ( -7.771249796623103556, -7.842167650704634063, 12.24886208192144998 ) ) ;
#7010 = CARTESIAN_POINT ( 'NONE',  ( 8.731428362939190890, -13.89598863503036164, 3.214285714285716633 ) ) ;
#7011 = CARTESIAN_POINT ( 'NONE',  ( 8.512513224245308763, 13.54758718765259040, 1.285714285714285809 ) ) ;
#7012 = CONTEXT_DEPENDENT_SHAPE_REPRESENTATION ( #9105, #7542 ) ;
#7013 = CARTESIAN_POINT ( 'NONE',  ( 13.55419868402807992, 4.742819248065649695, 43.92857142857143771 ) ) ;
#7014 = EDGE_CURVE ( 'NONE', #8307, #5716, #3987, .T. ) ;
#7015 = CARTESIAN_POINT ( 'NONE',  ( 1.478298951650704351, -14.28433602490913579, 37.64689771248358596 ) ) ;
#7016 = CARTESIAN_POINT ( 'NONE',  ( -9.383039235653820143, 1.486127417882155521, 8.700000000000041922 ) ) ;
#7017 = CARTESIAN_POINT ( 'NONE',  ( 1.737328882695370558, -14.25515036105620581, 41.63881657323070584 ) ) ;
#7018 = ORIENTED_EDGE ( 'NONE', *, *, #7907, .F. ) ;
#7019 = DIRECTION ( 'NONE',  ( -1.000000000000000000, 0.000000000000000000, 0.000000000000000000 ) ) ;
#7020 = CARTESIAN_POINT ( 'NONE',  ( 8.841785722321695573, -13.82664651025757152, 23.21024514465928235 ) ) ;
#7021 = B_SPLINE_CURVE_WITH_KNOTS ( 'NONE', 3,
 ( #3375, #4925, #6655, #1199, #2845, #9064, #2789, #3679, #1149, #4402, #3617, #4349, #475, #379, #6752, #9940, #4297, #5885, #5937, #5989, #3529, #322, #2075, #5224, #9169, #1972, #6605, #3569, #9838, #6812, #8329, #9989, #8170, #7609, #5125, #8378, #1301, #6039, #5071, #4453, #8222, #4248, #3469, #9793, #8277, #7502, #1923, #2740, #530, #1878, #426, #2895, #6700, #5026, #9117, #2022, #1105, #7399 ),
 .UNSPECIFIED., .F., .F.,
 ( 4, 2, 2, 2, 2, 2, 2, 2, 2, 2, 2, 2, 2, 2, 2, 2, 2, 2, 2, 2, 2, 2, 2, 2, 2, 2, 2, 2, 4 ),
 ( 0.01152039134867053824, 0.01353100581402706323, 0.01554162027938358823, 0.01755223474474011322, 0.01956284921009664168, 0.02157346367545316668, 0.02358407814080969514, 0.02458938537348795417, 0.02559469260616621666, 0.02609734622250534097, 0.02634867303067491007, 0.02647433643475969114, 0.02653716813680208342, 0.02659999983884447222, 0.02666283154088686450, 0.02672566324292925677, 0.02685132664701404132, 0.02710265345518360694, 0.02760530707152273819, 0.02861061430420100068, 0.02961592153687926665, 0.03162653600223580552, 0.03363715046759233745, 0.03464245770027060689, 0.03564776493294886939, 0.03966899386366194713, 0.04067430109634020963, 0.04167960832901848600, 0.04369022279437502487 ),
 .UNSPECIFIED. ) ;
#7022 = CARTESIAN_POINT ( 'NONE',  ( 11.60466159355861926, 11.60466159355874716, 1.500000000000003553 ) ) ;
#7023 = CARTESIAN_POINT ( 'NONE',  ( -4.270415729527831772, -8.486213763410670907, 6.098862081921437195 ) ) ;
#7024 = CARTESIAN_POINT ( 'NONE',  ( -5.404401153735176599, 15.06016580658422477, 20.42453085894499054 ) ) ;
#7025 = DIRECTION ( 'NONE',  ( -0.000000000000000000, 0.000000000000000000, 1.000000000000000000 ) ) ;
#7026 = CARTESIAN_POINT ( 'NONE',  ( -7.424621202458789426, 7.424621202458724589, 6.000000000000005329 ) ) ;
#7027 = FACE_OUTER_BOUND ( 'NONE', #6929, .T. ) ;
#7028 = FILL_AREA_STYLE_COLOUR ( '', #2926 ) ;
#7029 = VERTEX_POINT ( 'NONE', #4116 ) ;
#7030 = CARTESIAN_POINT ( 'NONE',  ( -1.665163862719845067, -15.91362231745477374, 47.85310228751642114 ) ) ;
#7031 = ORIENTED_EDGE ( 'NONE', *, *, #10208, .F. ) ;
#7032 = CARTESIAN_POINT ( 'NONE',  ( -1.642561882922479732, 10.37072757624896191, 6.299999999999972289 ) ) ;
#7033 = DIRECTION ( 'NONE',  ( 0.000000000000000000, 8.191099868251446680E-34, 1.000000000000000000 ) ) ;
#7034 = CARTESIAN_POINT ( 'NONE',  ( -12.22833218042443271, 7.529642458189139909, 31.78167371608784819 ) ) ;
#7035 = CARTESIAN_POINT ( 'NONE',  ( -9.377220287598998283, -4.724406229267462898, 1.401137918078568134 ) ) ;
#7036 = CARTESIAN_POINT ( 'NONE',  ( -1.612135949262737844, -9.858066664633888365, 6.951137918078597266 ) ) ;
#7037 = CARTESIAN_POINT ( 'NONE',  ( -162.8500000000000796, -0.2808225807418253672, 13.00000000000000533 ) ) ;
#7038 = CARTESIAN_POINT ( 'NONE',  ( -10.24623928997352351, -10.06191849875416899, 8.504040569626438284 ) ) ;
#7039 = CARTESIAN_POINT ( 'NONE',  ( -13.91197093850538380, -1.567502665446387278, 47.14285714285714590 ) ) ;
#7040 = VERTEX_POINT ( 'NONE', #7938 ) ;
#7041 = CARTESIAN_POINT ( 'NONE',  ( 16.32287076676382043, -1.707986654103810897, 10.35310228751642292 ) ) ;
#7043 = LINE ( 'NONE', #2347, #3630 ) ;
#7042 = CIRCLE ( 'NONE', #3415, 18.00000000000000355 ) ;
#7044 = CARTESIAN_POINT ( 'NONE',  ( -5.420364854931999155, -15.49051278174644253, 40.07142857142857650 ) ) ;
#7045 = FACE_BOUND ( 'NONE', #8690, .T. ) ;
#7046 = CARTESIAN_POINT ( 'NONE',  ( -158.0000000000000284, -6.938893903907228378E-15, 0.000000000000000000 ) ) ;
#7047 = CARTESIAN_POINT ( 'NONE',  ( -8.900167166472156666, 4.534861676072234893, 17.85000000000001918 ) ) ;
#7048 = CARTESIAN_POINT ( 'NONE',  ( 9.865911304835474738, 1.562606840307950051, 1.049999999999966738 ) ) ;
#7049 = FACE_OUTER_BOUND ( 'NONE', #7278, .T. ) ;
#7050 = CARTESIAN_POINT ( 'NONE',  ( 15.06016580658428694, -5.404401153735007846, 30.57546914105500946 ) ) ;
#7051 = DIRECTION ( 'NONE',  ( -1.000000000000000000, -0.000000000000000000, -0.000000000000000000 ) ) ;
#7052 = AXIS2_PLACEMENT_3D ( 'NONE', #1653, #3924, #5674 ) ;
#7053 = CARTESIAN_POINT ( 'NONE',  ( 5.543385399275644332, 15.44746603149420494, 29.07546914105501301 ) ) ;
#7054 = CARTESIAN_POINT ( 'NONE',  ( -1.791431617652833763, -15.89939535829188877, 21.85714285714286120 ) ) ;
#7055 = CARTESIAN_POINT ( 'NONE',  ( 9.147417256656757090, 12.88790924271200566, 48.73000000000002530 ) ) ;
#7056 = CARTESIAN_POINT ( 'NONE',  ( 8.731428362939190890, -13.89598863503036164, 9.214285714285717077 ) ) ;
#7057 = MANIFOLD_SOLID_BREP ( 'M4 Tapped Hole1', #4986 ) ;
#7058 = CARTESIAN_POINT ( 'NONE',  ( 1.689666864740335894, -10.36326688006720786, 8.798862081921429379 ) ) ;
#7059 = CARTESIAN_POINT ( 'NONE',  ( -11.31370849898482156, 11.31370849898469544, 5.999999999999998224 ) ) ;
#7060 = CARTESIAN_POINT ( 'NONE',  ( 11.31370849898482334, -11.31370849898469366, 9.000000000000001776 ) ) ;
#7061 = CARTESIAN_POINT ( 'NONE',  ( 1.607813917173037899, -14.26974319298267169, 45.64285714285715301 ) ) ;
#7062 = CARTESIAN_POINT ( 'NONE',  ( 4.865839792409144771, 13.51115193377589740, 35.07546914105501656 ) ) ;
#7063 = CARTESIAN_POINT ( 'NONE',  ( 9.383039235653818366, -1.486127417882131097, 13.19999999999998863 ) ) ;
#7064 = CARTESIAN_POINT ( 'NONE',  ( 7.806708723663831506, 7.806708723663931870, 18.74999999999998934 ) ) ;
#7065 = VERTEX_POINT ( 'NONE', #812 ) ;
#7066 = CARTESIAN_POINT ( 'NONE',  ( 13.21436662431716869, -4.623906867372263640, 2.571428571428571619 ) ) ;
#7067 = DIRECTION ( 'NONE',  ( 0.000000000000000000, -8.191099868251446680E-34, -1.000000000000000000 ) ) ;
#7068 = ORIENTED_EDGE ( 'NONE', *, *, #8641, .F. ) ;
#7069 = PLANE ( 'NONE',  #6293 ) ;
#7070 = CARTESIAN_POINT ( 'NONE',  ( 8.404922754268618235, 13.61519076058357491, 27.28167371608785174 ) ) ;
#7071 = CARTESIAN_POINT ( 'NONE',  ( 8.512513224245308763, 13.54758718765259040, 1.285714285714285809 ) ) ;
#7072 = CARTESIAN_POINT ( 'NONE',  ( 16.32287076676382043, -1.707986654103810897, 22.35310228751642114 ) ) ;
#7073 = DIRECTION ( 'NONE',  ( -0.000000000000000000, 1.000000000000000000, 1.224646799147353207E-16 ) ) ;
#7074 = CARTESIAN_POINT ( 'NONE',  ( 7.806708723663831506, 7.806708723663930982, 6.749999999999960032 ) ) ;
#7075 = CARTESIAN_POINT ( 'NONE',  ( -68.00000000000001421, 0.000000000000000000, 8.500000000000000000 ) ) ;
#7076 = SURFACE_STYLE_FILL_AREA ( #3102 ) ;
#7077 = MANIFOLD_SOLID_BREP ( 'Cavity1', #2342 ) ;
#7078 = CARTESIAN_POINT ( 'NONE',  ( -8.512513224245306986, -13.54758718765259218, 34.28571428571428470 ) ) ;
#7079 = ORIENTED_EDGE ( 'NONE', *, *, #8669, .T. ) ;
#7080 = CARTESIAN_POINT ( 'NONE',  ( -4.766900247265192014, -9.355568503977876205, 5.099999999999993427 ) ) ;
#7081 = CARTESIAN_POINT ( 'NONE',  ( -5.420364854931999155, -15.49051278174644253, 10.07142857142856940 ) ) ;
#7082 = DIRECTION ( 'NONE',  ( -1.000000000000000000, 1.842239752758738928E-31, -1.780435181894459419E-32 ) ) ;
#7083 = CARTESIAN_POINT ( 'NONE',  ( -11.78653521626494793, -7.556039541191465148, 24.71024514465928235 ) ) ;
#7084 = CARTESIAN_POINT ( 'NONE',  ( 1.776620879821457333, 10.89658364409028124, 5.451137918078557298 ) ) ;
#7085 = CARTESIAN_POINT ( 'NONE',  ( -8.877401133907129704, 4.579542530753038854, 16.85113791807854611 ) ) ;
#7086 = LINE ( 'NONE', #6355, #4467 ) ;
#7087 = CARTESIAN_POINT ( 'NONE',  ( -14.25515036105622890, 1.737328882695209575, 3.361183426769288385 ) ) ;
#7088 = AXIS2_PLACEMENT_3D ( 'NONE', #3176, #3225, #6312 ) ;
#7089 = CARTESIAN_POINT ( 'NONE',  ( 14.25515036105622535, -1.737328882695210241, 18.36118342676929771 ) ) ;
#7090 = VERTEX_POINT ( 'NONE', #8829 ) ;
#7091 = CARTESIAN_POINT ( 'NONE',  ( 15.44746603149413922, 5.543385399275817527, 3.924530858944990541 ) ) ;
#7092 = FACE_OUTER_BOUND ( 'NONE', #2576, .T. ) ;
#7093 = CARTESIAN_POINT ( 'NONE',  ( -13.89598863503046111, 8.731428362939027465, 47.78571428571430602 ) ) ;
#7094 = DIRECTION ( 'NONE',  ( 0.000000000000000000, -6.338944243255235518E-49, 1.000000000000000000 ) ) ;
#7095 = AXIS2_PLACEMENT_3D ( 'NONE', #1695, #7213, #763 ) ;
#7096 = CARTESIAN_POINT ( 'NONE',  ( -8.464561979789474222, -4.312909747525729642, 14.39999999999996838 ) ) ;
#7097 = CARTESIAN_POINT ( 'NONE',  ( -9.865911304835474738, -1.562606840307925626, 8.549999999999963407 ) ) ;
#7098 = LINE ( 'NONE', #656, #1995 ) ;
#7099 = CARTESIAN_POINT ( 'NONE',  ( -5.164528828830334817, 15.14410076328347543, 22.43261199819786356 ) ) ;
#7100 = CYLINDRICAL_SURFACE ( 'NONE', #336, 8.200000000000001066 ) ;
#7101 = CARTESIAN_POINT ( 'NONE',  ( -15.53355953199861794, -5.297344310588530725, 38.93261199819787777 ) ) ;
#7102 = AXIS2_PLACEMENT_3D ( 'NONE', #3488, #6001, #2753 ) ;
#7103 = CIRCLE ( 'NONE', #339, 8.200000000000001066 ) ;
#7104 = VERTEX_POINT ( 'NONE', #4317 ) ;
#7105 = EDGE_CURVE ( 'NONE', #7562, #913, #8776, .T. ) ;
#7106 = CIRCLE ( 'NONE', #531, 0.9906000000000003691 ) ;
#7107 = CARTESIAN_POINT ( 'NONE',  ( 15.89939535829187278, 1.791431617653015174, 20.14285714285714235 ) ) ;
#7108 = DIRECTION ( 'NONE',  ( 0.000000000000000000, 0.000000000000000000, 1.000000000000000000 ) ) ;
#7109 = VERTEX_POINT ( 'NONE', #4367 ) ;
#7110 = CARTESIAN_POINT ( 'NONE',  ( 5.420364854932001819, 15.49051278174644430, 1.071428571428570287 ) ) ;
#7111 = EDGE_CURVE ( 'NONE', #7847, #7040, #849, .T. ) ;
#7112 = FILL_AREA_STYLE_COLOUR ( '', #16 ) ;
#7113 = DIRECTION ( 'NONE',  ( 1.000000000000000000, 0.000000000000000000, 0.000000000000000000 ) ) ;
#7114 = COLOUR_RGB ( '', 0.31764706, 0.68627451, 0.89019608) ;
#7115 = AXIS2_PLACEMENT_3D ( 'NONE', #269, #3522, #3416 ) ;
#7116 = PRODUCT_DEFINITION_CONTEXT ( 'detailed design', #451, 'design' ) ;
#7117 = MANIFOLD_SOLID_BREP ( 'M4 Clearance Hole1', #5799 ) ;
#7118 = CARTESIAN_POINT ( 'NONE',  ( -1.677562661911643938, -10.91227292449344688, 11.94886208192145993 ) ) ;
#7119 = CARTESIAN_POINT ( 'NONE',  ( 13.82664651025767100, -8.841785722321541030, 0.7897548553407187644 ) ) ;
#7120 = CARTESIAN_POINT ( 'NONE',  ( -16.30827793483735988, 1.837501619626141780, 17.35714285714286476 ) ) ;
#7121 = CARTESIAN_POINT ( 'NONE',  ( -9.899494936611716867, 9.899494936611610285, 36.00000000000000711 ) ) ;
#7122 = APPLICATION_CONTEXT ( 'automotive_design' ) ;
#7123 = CARTESIAN_POINT ( 'NONE',  ( 1.478298951650704351, -14.28433602490913579, 31.64689771248358241 ) ) ;
#7124 = CARTESIAN_POINT ( 'NONE',  ( -8.464561979789474222, -4.312909747525729642, 8.399999999999963052 ) ) ;
#7125 = CARTESIAN_POINT ( 'NONE',  ( -7.771249796623103556, -7.842167650704637616, 3.248862081921429112 ) ) ;
#7126 = EDGE_LOOP ( 'NONE', ( #3935, #3975, #6373, #6173, #1209, #673 ) ) ;
#7127 = CARTESIAN_POINT ( 'NONE',  ( -14.28433602490915000, 1.478298951650542481, 49.35310228751642114 ) ) ;
#7128 = EDGE_CURVE ( 'NONE', #5864, #7530, #8261, .T. ) ;
#7129 = DIRECTION ( 'NONE',  ( 0.000000000000000000, -6.338944243255235518E-49, 1.000000000000000000 ) ) ;
#7130 = CARTESIAN_POINT ( 'NONE',  ( -11.40355824106246807, 11.22385875690704715, 31.99595943037357060 ) ) ;
#7131 = CARTESIAN_POINT ( 'NONE',  ( -1.791431617652833763, -15.89939535829188877, 15.85714285714286120 ) ) ;
#7132 = CARTESIAN_POINT ( 'NONE',  ( 15.44746603149413922, 5.543385399275817527, 21.92453085894500120 ) ) ;
#7133 = CARTESIAN_POINT ( 'NONE',  ( 1.642561882922480621, -10.37072757624892638, 1.800000000000023803 ) ) ;
#7134 = CARTESIAN_POINT ( 'NONE',  ( 9.355568503977840678, 4.766900247265305701, 0.9000000000000119016 ) ) ;
#7135 = CARTESIAN_POINT ( 'NONE',  ( -31.74999999999994316, 4.286263797015736595E-16, -3.500000000000000000 ) ) ;
#7136 = DIRECTION ( 'NONE',  ( 0.000000000000000000, 0.000000000000000000, -1.000000000000000000 ) ) ;
#7137 = EDGE_LOOP ( 'NONE', ( #4002, #8251, #505, #2788 ) ) ;
#7138 = CARTESIAN_POINT ( 'NONE',  ( -7.806708723663831506, -7.806708723663902560, 17.25000000000003197 ) ) ;
#7139 = CARTESIAN_POINT ( 'NONE',  ( -16.30827793483735988, 1.837501619626141780, 11.35714285714285943 ) ) ;
#7140 = CYLINDRICAL_SURFACE ( 'NONE', #9321, 13.00000000000000355 ) ;
#7141 = CARTESIAN_POINT ( 'NONE',  ( 9.989344678689365153, -9.809645194533958446, 28.99595943037357060 ) ) ;
#7142 = CARTESIAN_POINT ( 'NONE',  ( 1.776620879821457333, 10.89658364409028124, 8.451137918078549305 ) ) ;
#7143 = CARTESIAN_POINT ( 'NONE',  ( 4.355403765523470305, 8.442910196168364578, 11.60113791807856742 ) ) ;
#7144 = DIRECTION ( 'NONE',  ( -1.000000000000000000, -0.000000000000000000, -0.000000000000000000 ) ) ;
#7145 = CARTESIAN_POINT ( 'NONE',  ( 14.25515036105622535, -1.737328882695210241, 12.36118342676929771 ) ) ;
#7146 = TOROIDAL_SURFACE ( 'NONE', #7474, 8.000000000000000000, 1.000000000000000888 ) ;
#7147 = CARTESIAN_POINT ( 'NONE',  ( -4.503970704919988854, 13.25633410266674517, 10.43261199819786356 ) ) ;
#7148 = ORIENTED_EDGE ( 'NONE', *, *, #9435, .T. ) ;
#7149 = VECTOR ( 'NONE', #6716, 1000.000000000000000 ) ;
#7150 = DIRECTION ( 'NONE',  ( -4.818676322157796389E-17, 1.000000000000000000, 0.000000000000000000 ) ) ;
#7151 = EDGE_CURVE ( 'NONE', #3042, #9714, #2323, .T. ) ;
#7152 = CARTESIAN_POINT ( 'NONE',  ( -1.967016585148659846, 16.29368510291087091, 2.638816573230710727 ) ) ;
#7153 = CARTESIAN_POINT ( 'NONE',  ( 9.934157114783658926, 9.864832758439671778, 48.73000000000001819 ) ) ;
#7154 = CARTESIAN_POINT ( 'NONE',  ( -1.562606840307830591, -9.865911304835478290, 16.94999999999998863 ) ) ;
#7155 = CARTESIAN_POINT ( 'NONE',  ( 9.383039235653818366, -1.486127417882129986, 7.199999999999984190 ) ) ;
#7156 = CARTESIAN_POINT ( 'NONE',  ( 14.00000000000000533, 2.210487472460973684E-16, -1.610000000000000098 ) ) ;
#7157 = CARTESIAN_POINT ( 'NONE',  ( 5.543385399275644332, 15.44746603149420494, 29.07546914105501301 ) ) ;
#7158 = CARTESIAN_POINT ( 'NONE',  ( -31.74999999999994316, 0.000000000000000000, 0.000000000000000000 ) ) ;
#7159 = CARTESIAN_POINT ( 'NONE',  ( 5.164528828830335705, -15.14410076328347543, 37.43261199819787066 ) ) ;
#7160 = VERTEX_POINT ( 'NONE', #7467 ) ;
#7161 = CARTESIAN_POINT ( 'NONE',  ( -8.512513224245306986, -13.54758718765259218, 34.28571428571428470 ) ) ;
#7162 = CARTESIAN_POINT ( 'NONE',  ( 2.000000000000001776, 0.000000000000000000, 0.000000000000000000 ) ) ;
#7163 = CARTESIAN_POINT ( 'NONE',  ( -13.54758718765249625, -8.512513224245459753, 4.714285714285712636 ) ) ;
#7164 = CARTESIAN_POINT ( 'NONE',  ( -6.751237864895158758, 6.683790977649260334, 0.9988620819214170110 ) ) ;
#7165 = AXIS2_PLACEMENT_3D ( 'NONE', #157, #6453, #8063 ) ;
#7166 = CARTESIAN_POINT ( 'NONE',  ( 10.37818827243067510, -1.595456901104499448, 14.19886208192146171 ) ) ;
#7167 = CARTESIAN_POINT ( 'NONE',  ( -5.164528828830334817, 15.14410076328347543, -1.567388001802134223 ) ) ;
#7168 = CARTESIAN_POINT ( 'NONE',  ( 11.60466159355862104, 11.60466159355875071, 19.50000000000000355 ) ) ;
#7169 = CARTESIAN_POINT ( 'NONE',  ( -7.448449071214644945, -11.85413878919601771, 34.28571428571428470 ) ) ;
#7170 = CARTESIAN_POINT ( 'NONE',  ( 9.989344678689260348, 9.809645194534072132, 47.50404056962644006 ) ) ;
#7171 = EDGE_CURVE ( 'NONE', #7728, #9896, #2163, .T. ) ;
#7172 = CARTESIAN_POINT ( 'NONE',  ( -11.85413878919593422, -7.448449071214776396, 4.714285714285712636 ) ) ;
#7173 = CARTESIAN_POINT ( 'NONE',  ( -9.383039235653820143, 1.486127417882155299, 17.69999999999999218 ) ) ;
#7174 = CARTESIAN_POINT ( 'NONE',  ( -5.012215536711506658, 9.837026868206022456, 18.15000000000000924 ) ) ;
#7175 = ORIENTED_EDGE ( 'NONE', *, *, #4241, .F. ) ;
#7176 = CARTESIAN_POINT ( 'NONE',  ( 11.85413878919593422, 7.448449071214774619, 1.714285714285716855 ) ) ;
#7177 = ORIENTED_EDGE ( 'NONE', *, *, #987, .T. ) ;
#7178 = DIRECTION ( 'NONE',  ( -1.000000000000000000, -0.000000000000000000, -0.000000000000000000 ) ) ;
#7179 = EDGE_CURVE ( 'NONE', #5232, #2003, #2816, .T. ) ;
#7180 = CARTESIAN_POINT ( 'NONE',  ( -15.89939535829186923, -1.791431617653016062, 23.14285714285714590 ) ) ;
#7181 = CARTESIAN_POINT ( 'NONE',  ( -15.88516839912898071, -1.917699372586004980, 43.13881657323070584 ) ) ;
#7182 = APPLICATION_CONTEXT ( 'automotive_design' ) ;
#7183 = PLANE ( 'NONE',  #8415 ) ;
#7184 = CARTESIAN_POINT ( 'NONE',  ( -7.424621202458789426, 7.424621202458720148, 3.000000000000002665 ) ) ;
#7185 = CARTESIAN_POINT ( 'NONE',  ( -1.607813917173034124, 14.26974319298267346, 0.6428571428571433488 ) ) ;
#7186 = ORIENTED_EDGE ( 'NONE', *, *, #7487, .F. ) ;
#7187 = CARTESIAN_POINT ( 'NONE',  ( 14.28433602490915000, -1.478298951650544479, 16.35310228751641759 ) ) ;
#7188 = CARTESIAN_POINT ( 'NONE',  ( 4.766900247265192903, 9.355568503977902850, 15.60000000000000320 ) ) ;
#7189 = CARTESIAN_POINT ( 'NONE',  ( -1.791431617652833763, -15.89939535829188877, 15.85714285714286120 ) ) ;
#7190 = DIRECTION ( 'NONE',  ( -1.000000000000000000, 1.842239752758738928E-31, -1.780435181894459419E-32 ) ) ;
#7191 = CARTESIAN_POINT ( 'NONE',  ( 9.377220287599001836, 4.724406229267492208, 2.901137918078569466 ) ) ;
#7192 = CARTESIAN_POINT ( 'NONE',  ( 1.439022436064387511, -9.390499931835517344, 12.80113791807860224 ) ) ;
#7193 = CARTESIAN_POINT ( 'NONE',  ( -58.00000000000002842, 1.249000902703378268E-16, 18.00000000000002132 ) ) ;
#7194 = B_SPLINE_CURVE_WITH_KNOTS ( 'NONE', 3,
 ( #6760, #6611, #5185, #9946, #3479, #7405, #4458, #4256, #7558, #8334, #5078, #5843, #8228, #2796, #5945, #6661, #9843, #2081, #1156, #2746, #9125, #5891, #9070, #5229, #1306, #3685, #8178, #9744, #2650, #1979 ),
 .UNSPECIFIED., .F., .F.,
 ( 4, 2, 2, 2, 2, 2, 2, 2, 2, 2, 2, 2, 2, 2, 4 ),
 ( 4.816881890085070803E-18, 0.0004206592251581338219, 0.0008413184503162626565, 0.001261977675474391545, 0.001682636900632520326, 0.002523955350948835566, 0.003365273801265151240, 0.003785933026423350060, 0.004206592251581550181, 0.004627251476739749000, 0.005047910701897948688, 0.005468569927056148375, 0.005889229152214347195, 0.006309888377372546882, 0.006730547602530746569 ),
 .UNSPECIFIED. ) ;
#7195 = CARTESIAN_POINT ( 'NONE',  ( 11.92174236212692229, 7.340858601238088532, -0.2816737160878517443 ) ) ;
#7196 = CARTESIAN_POINT ( 'NONE',  ( 4.865839792409144771, 13.51115193377589740, 17.07546914105500591 ) ) ;
#7197 = ORIENTED_EDGE ( 'NONE', *, *, #9018, .F. ) ;
#7198 = DIRECTION ( 'NONE',  ( 0.000000000000000000, 1.000000000000000000, 1.224646799147353207E-16 ) ) ;
#7199 = CARTESIAN_POINT ( 'NONE',  ( 13.54758718765249803, 8.512513224245457977, 43.71428571428572241 ) ) ;
#7200 = CARTESIAN_POINT ( 'NONE',  ( -164.1743453116437763, -1.432625545945890311, 12.92095975507885441 ) ) ;
#7201 = DIRECTION ( 'NONE',  ( 0.000000000000000000, -1.000000000000000000, 0.000000000000000000 ) ) ;
#7202 = CARTESIAN_POINT ( 'NONE',  ( -9.383039235653820143, 1.486127417882155299, 17.69999999999999218 ) ) ;
#7203 = CARTESIAN_POINT ( 'NONE',  ( 7.063212654743467489, 7.063212654743553642, 9.749999999999982236 ) ) ;
#7204 = CARTESIAN_POINT ( 'NONE',  ( 7.071067811865515473, -7.071067811865425767, 19.50000000000001776 ) ) ;
#7205 = CARTESIAN_POINT ( 'NONE',  ( 11.69682198916835070, 11.51250119794901394, 29.50404056962643295 ) ) ;
#7206 = DIRECTION ( 'NONE',  ( -1.000000000000000000, 0.000000000000000000, 0.000000000000000000 ) ) ;
#7207 = CARTESIAN_POINT ( 'NONE',  ( -13.82664651025767100, 8.841785722321537477, 27.78975485534072121 ) ) ;
#7208 = AXIS2_PLACEMENT_3D ( 'NONE', #5874, #9930, #5778 ) ;
#7209 = ORIENTED_EDGE ( 'NONE', *, *, #585, .F. ) ;
#7210 = CARTESIAN_POINT ( 'NONE',  ( -13.54758718765249625, -8.512513224245459753, 28.71428571428571530 ) ) ;
#7211 = CARTESIAN_POINT ( 'NONE',  ( 3.824282371705687744, 14.64065971923091602, 7.152024097632292178E-17 ) ) ;
#7212 = ORIENTED_EDGE ( 'NONE', *, *, #4270, .F. ) ;
#7213 = DIRECTION ( 'NONE',  ( -1.000000000000000000, -0.000000000000000000, -0.000000000000000000 ) ) ;
#7214 = CARTESIAN_POINT ( 'NONE',  ( -7.771249796623103556, -7.842167650704634063, 15.24886208192144110 ) ) ;
#7215 = AXIS2_PLACEMENT_3D ( 'NONE', #8417, #2324, #5474 ) ;
#7216 = UNCERTAINTY_MEASURE_WITH_UNIT (LENGTH_MEASURE( 1.000000000000000082E-05 ), #620, 'distance_accuracy_value', 'NONE');
#7217 = CARTESIAN_POINT ( 'NONE',  ( -13.59724543428031573, -4.619798703722008959, 44.93261199819787777 ) ) ;
#7218 = CARTESIAN_POINT ( 'NONE',  ( -15.89939535829186923, -1.791431617653016062, 17.14285714285713880 ) ) ;
#7219 = CARTESIAN_POINT ( 'NONE',  ( 7.448449071214646722, 11.85413878919601594, 43.28571428571429180 ) ) ;
#7220 = CARTESIAN_POINT ( 'NONE',  ( -12.08964793087886314, 7.750357176954159932, 39.78975485534073186 ) ) ;
#7221 = EDGE_CURVE ( 'NONE', #3552, #4954, #7519, .T. ) ;
#7222 = CARTESIAN_POINT ( 'NONE',  ( -13.91197093850538380, -1.567502665446387278, 5.142857142857143238 ) ) ;
#7223 = CARTESIAN_POINT ( 'NONE',  ( -6.717514421272238856, 6.717514421272180236, 15.00000000000001421 ) ) ;
#7224 = CARTESIAN_POINT ( 'NONE',  ( 10.89658364409024749, 1.776620879821585897, 11.04886208192144359 ) ) ;
#7225 = ORIENTED_EDGE ( 'NONE', *, *, #3604, .F. ) ;
#7226 = CARTESIAN_POINT ( 'NONE',  ( -13.89774397934249706, -1.693770420379375974, 49.13881657323070584 ) ) ;
#7227 = CARTESIAN_POINT ( 'NONE',  ( -158.0000000000000284, -18.00000000000001066, 2.204364238465236217E-15 ) ) ;
#7228 = CARTESIAN_POINT ( 'NONE',  ( 5.420364854932000931, 15.49051278174644075, 19.07142857142856940 ) ) ;
#7229 = CARTESIAN_POINT ( 'NONE',  ( -13.96533075980324234, 8.621071003556515677, 31.78167371608784819 ) ) ;
#7230 = CARTESIAN_POINT ( 'NONE',  ( 9.355568503977840678, 4.766900247265305701, 12.90000000000002345 ) ) ;
#7231 = CARTESIAN_POINT ( 'NONE',  ( 7.424621202458790314, -7.424621202458697944, 7.500000000000007105 ) ) ;
#7232 = CARTESIAN_POINT ( 'NONE',  ( 1.567502665446232957, 13.91197093850540156, 0.8571428571428549859 ) ) ;
#7233 = AXIS2_PLACEMENT_3D ( 'NONE', #33, #9244, #1390 ) ;
#7234 = ADVANCED_FACE ( 'NONE', ( #2809, #291 ), #2038, .T. ) ;
#7235 = ORIENTED_EDGE ( 'NONE', *, *, #8845, .F. ) ;
#7236 = CARTESIAN_POINT ( 'NONE',  ( 7.340858601237956194, 11.92174236212700045, 15.28167371608785174 ) ) ;
#7237 = CARTESIAN_POINT ( 'NONE',  ( 7.806708723663832394, 7.806708723663926541, 9.749999999999982236 ) ) ;
#7238 = CYLINDRICAL_SURFACE ( 'NONE', #7165, 13.00000000000001243 ) ;
#7239 = CARTESIAN_POINT ( 'NONE',  ( 15.49051278174638036, 5.420364854932175014, 37.92857142857143060 ) ) ;
#7240 = CARTESIAN_POINT ( 'NONE',  ( 1.441234910513245149, 13.92619789766829008, 44.85310228751641404 ) ) ;
#7241 = CARTESIAN_POINT ( 'NONE',  ( -7.390897758835869524, 7.458344646081644491, 17.00113791807859442 ) ) ;
#7242 = CARTESIAN_POINT ( 'NONE',  ( -9.873755945037078874, -1.513077731353020594, 16.55113791807855605 ) ) ;
#7243 = DIRECTION ( 'NONE',  ( 0.000000000000000000, 0.000000000000000000, 1.000000000000000000 ) ) ;
#7244 = CARTESIAN_POINT ( 'NONE',  ( 7.556039541191335474, 11.78653521626503320, 23.28975485534072121 ) ) ;
#7245 = CARTESIAN_POINT ( 'NONE',  ( -10.24623928997352351, -10.06191849875416899, 8.504040569626438284 ) ) ;
#7246 = CARTESIAN_POINT ( 'NONE',  ( 5.986002070941135678, -13.58603705635637304, -1.270000000000007123 ) ) ;
#7247 = CARTESIAN_POINT ( 'NONE',  ( -16.32287076676382398, 1.707986654103809343, 13.35310228751641937 ) ) ;
#7248 = FACE_OUTER_BOUND ( 'NONE', #8416, .T. ) ;
#7249 = DIRECTION ( 'NONE',  ( -1.000000000000000000, -0.000000000000000000, -0.000000000000000000 ) ) ;
#7250 = CARTESIAN_POINT ( 'NONE',  ( 9.375578539472099848, -1.533232399699987702, 0.2011379180785754783 ) ) ;
#7251 = CARTESIAN_POINT ( 'NONE',  ( -4.534861676072319270, 8.900167166472122915, 9.150000000000003908 ) ) ;
#7252 = PRODUCT_DEFINITION ( 'UNKNOWN', '', #6887, #8346 ) ;
#7253 = CARTESIAN_POINT ( 'NONE',  ( -167.1500000000000341, -5.483569848023176209E-15, 13.00000000000000178 ) ) ;
#7254 = CARTESIAN_POINT ( 'NONE',  ( 1.917699372585825790, 15.88516839912900203, 28.86118342676929416 ) ) ;
#7255 = CARTESIAN_POINT ( 'NONE',  ( -1.562606840307830591, -9.865911304835481843, 1.949999999999996403 ) ) ;
#7256 = CARTESIAN_POINT ( 'NONE',  ( -5.543385399275643444, -15.44746603149420494, 32.07546914105502367 ) ) ;
#7257 = ORIENTED_EDGE ( 'NONE', *, *, #2535, .T. ) ;
#7258 = VECTOR ( 'NONE', #7206, 1000.000000000000000 ) ;
#7259 = CARTESIAN_POINT ( 'NONE',  ( 15.49051278174638036, 5.420364854932175014, 37.92857142857143060 ) ) ;
#7260 = LINE ( 'NONE', #5039, #6265 ) ;
#7261 = CARTESIAN_POINT ( 'NONE',  ( 15.10213328493390783, -5.284464991282587398, 20.57142857142857295 ) ) ;
#7262 =( LENGTH_UNIT ( ) NAMED_UNIT ( * ) SI_UNIT ( .MILLI., .METRE. ) );
#7263 = CARTESIAN_POINT ( 'NONE',  ( 6.751237864895159646, -6.683790977649239906, 11.49886208192146775 ) ) ;
#7264 = CARTESIAN_POINT ( 'NONE',  ( 9.333916720356675967, 4.809394265263123636, 19.89886208192141481 ) ) ;
#7265 = CARTESIAN_POINT ( 'NONE',  ( -12.08964793087886314, 7.750357176954159932, 39.78975485534073186 ) ) ;
#7266 = VECTOR ( 'NONE', #487, 1000.000000000000000 ) ;
#7267 = CARTESIAN_POINT ( 'NONE',  ( 15.10213328493390783, -5.284464991282587398, 14.57142857142856940 ) ) ;
#7268 = AXIS2_PLACEMENT_3D ( 'NONE', #7295, #2543, #5687 ) ;
#7269 = DIRECTION ( 'NONE',  ( 1.000000000000000000, 0.000000000000000000, 0.000000000000000000 ) ) ;
#7270 = CARTESIAN_POINT ( 'NONE',  ( 8.620103694221997515, 13.47998361472160767, -0.7102451446592792372 ) ) ;
#7271 = ADVANCED_FACE ( 'NONE', ( #2659 ), #3389, .T. ) ;
#7272 = CARTESIAN_POINT ( 'NONE',  ( 9.899494936611718643, -9.899494936611608509, 9.000000000000001776 ) ) ;
#7273 = CARTESIAN_POINT ( 'NONE',  ( 4.534861676072321046, -8.900167166472098046, 16.64999999999999858 ) ) ;
#7274 = CARTESIAN_POINT ( 'NONE',  ( 9.333916720356675967, 4.809394265263126300, 7.898862081921404155 ) ) ;
#7275 = ORIENTED_EDGE ( 'NONE', *, *, #6522, .F. ) ;
#7276 = CARTESIAN_POINT ( 'NONE',  ( -14.26974319298268767, 1.607813917172874918, 5.357142857142856762 ) ) ;
#7277 = ADVANCED_FACE ( 'NONE', ( #1893 ), #5042, .T. ) ;
#7278 = EDGE_LOOP ( 'NONE', ( #9525, #8525, #1084, #2243 ) ) ;
#7279 = CIRCLE ( 'NONE', #9600, 13.00000000000000000 ) ;
#7280 = DIRECTION ( 'NONE',  ( -1.000000000000000000, 1.842239752758738928E-31, -1.780435181894459419E-32 ) ) ;
#7281 = AXIS2_PLACEMENT_3D ( 'NONE', #4343, #9007, #1918 ) ;
#7282 = EDGE_CURVE ( 'NONE', #6243, #4850, #5851, .T. ) ;
#7283 = CARTESIAN_POINT ( 'NONE',  ( 1.791431617652837316, 15.89939535829188877, 12.85714285714285943 ) ) ;
#7284 = CARTESIAN_POINT ( 'NONE',  ( -1.967016585148659846, 16.29368510291087091, 38.63881657323070584 ) ) ;
#7285 = CARTESIAN_POINT ( 'NONE',  ( 7.424621202458790314, -7.424621202458697944, 7.500000000000007105 ) ) ;
#7286 = CARTESIAN_POINT ( 'NONE',  ( -7.806708723663830618, -7.806708723663902560, 14.25000000000001243 ) ) ;
#7287 = DIRECTION ( 'NONE',  ( -1.000000000000000000, -0.000000000000000000, -0.000000000000000000 ) ) ;
#7288 = COLOUR_RGB ( '', 0.09019608, 0.27058824, 0.51372549) ;
#7289 = CARTESIAN_POINT ( 'NONE',  ( -1.737328882695368115, 14.25515036105620581, 14.63881657323070939 ) ) ;
#7290 = CARTESIAN_POINT ( 'NONE',  ( 1.727091770866551412, 10.90442828429187117, 12.44999999999995666 ) ) ;
#7291 = CARTESIAN_POINT ( 'NONE',  ( -163.3500000000000512, -1.154202410357457390E-14, 13.00000000000000355 ) ) ;
#7292 = CARTESIAN_POINT ( 'NONE',  ( 9.989344678689365153, -9.809645194533958446, 34.99595943037355994 ) ) ;
#7293 = CARTESIAN_POINT ( 'NONE',  ( 10.91227292449344155, 1.677562661911773390, 15.05113791807855961 ) ) ;
#7294 = CARTESIAN_POINT ( 'NONE',  ( 7.098671581784200768, 7.027753727702831021, 11.75113791807857666 ) ) ;
#7295 = CARTESIAN_POINT ( 'NONE',  ( -5.986002070941133901, -13.58603705635637304, -1.270000000000007123 ) ) ;
#7296 = CARTESIAN_POINT ( 'NONE',  ( -11.92174236212692051, -7.340858601238089420, 14.71832628391215003 ) ) ;
#7297 = ADVANCED_FACE ( 'NONE', ( #5089 ), #2860, .T. ) ;
#7298 = CARTESIAN_POINT ( 'NONE',  ( -13.59724543428031573, -4.619798703722008959, 14.93261199819787066 ) ) ;
#7299 = ORIENTED_EDGE ( 'NONE', *, *, #2228, .F. ) ;
#7300 = DIRECTION ( 'NONE',  ( 0.000000000000000000, -6.338944243255235518E-49, 1.000000000000000000 ) ) ;
#7301 = CARTESIAN_POINT ( 'NONE',  ( 11.51250119794888249, 11.69682198916847682, 3.495959430373559940 ) ) ;
#7302 = FACE_OUTER_BOUND ( 'NONE', #3183, .T. ) ;
#7303 = DIRECTION ( 'NONE',  ( -1.000000000000000000, 1.842239752758738928E-31, -1.780435181894459419E-32 ) ) ;
#7304 = CARTESIAN_POINT ( 'NONE',  ( 6.683790977649321619, -6.751237864895076157, 6.501137918078588207 ) ) ;
#7305 = CARTESIAN_POINT ( 'NONE',  ( 9.865911304835474738, 1.562606840307948719, 4.049999999999988276 ) ) ;
#7306 = CARTESIAN_POINT ( 'NONE',  ( -167.0812335317077668, 0.5573535649547497473, 12.98877602732082615 ) ) ;
#7307 = B_SPLINE_CURVE_WITH_KNOTS ( 'NONE', 3,
 ( #3455, #3666, #2779, #6739, #9931, #9782, #1140, #2835, #4286, #5875, #2683, #5827, #9003, #5927 ),
 .UNSPECIFIED., .F., .F.,
 ( 4, 2, 2, 2, 2, 2, 4 ),
 ( 0.000000000000000000, 0.001440048918583816629, 0.002880097837167633259, 0.005760195674335269987, 0.007200244592919087701, 0.008640293511502904547, 0.01152039134867053824 ),
 .UNSPECIFIED. ) ;
#7308 = CARTESIAN_POINT ( 'NONE',  ( 14.26974319298268767, -1.607813917172876916, 26.35714285714285765 ) ) ;
#7309 = CARTESIAN_POINT ( 'NONE',  ( 1.917699372585825790, 15.88516839912900203, 40.86118342676929416 ) ) ;
#7310 = EDGE_LOOP ( 'NONE', ( #7275, #44 ) ) ;
#7311 = CARTESIAN_POINT ( 'NONE',  ( 5.284464991282756152, -15.10213328493384743, 33.42857142857143060 ) ) ;
#7312 = CARTESIAN_POINT ( 'NONE',  ( -6.139641135253190107, 12.65605934851316228, 2.357314452189447182E-16 ) ) ;
#7313 = EDGE_CURVE ( 'NONE', #8249, #9073, #7603, .T. ) ;
#7314 = CARTESIAN_POINT ( 'NONE',  ( 1.837501619626330074, -16.30827793483733501, 15.64285714285714235 ) ) ;
#7315 =( REPRESENTATION_RELATIONSHIP ('NONE','NONE', #58, #3478 ) REPRESENTATION_RELATIONSHIP_WITH_TRANSFORMATION ( #7945 )SHAPE_REPRESENTATION_RELATIONSHIP( ) );
#7316 = CARTESIAN_POINT ( 'NONE',  ( -158.0000000000000284, 14.99999999999999289, 0.000000000000000000 ) ) ;
#7317 = CARTESIAN_POINT ( 'NONE',  ( 1.486127417882244783, -9.383039235653791721, 1.800000000000023803 ) ) ;
#7318 = CARTESIAN_POINT ( 'NONE',  ( 9.859792900771104485, -4.967534682030585458, 17.34886208192141765 ) ) ;
#7319 = UNCERTAINTY_MEASURE_WITH_UNIT (LENGTH_MEASURE( 1.000000000000000082E-05 ), #1172, 'distance_accuracy_value', 'NONE');
#7320 = CARTESIAN_POINT ( 'NONE',  ( 9.989344678689260348, 9.809645194534072132, 47.50404056962644006 ) ) ;
#7321 = CARTESIAN_POINT ( 'NONE',  ( 16.30827793483735633, -1.837501619626142890, 32.35714285714286120 ) ) ;
#7322 = CARTESIAN_POINT ( 'NONE',  ( -10.15407889436378852, -10.15407889436390398, 46.50000000000001421 ) ) ;
#7323 = CARTESIAN_POINT ( 'NONE',  ( 13.92619789766827587, 1.441234910513398582, 36.14689771248357886 ) ) ;
#7324 = CARTESIAN_POINT ( 'NONE',  ( -7.448449071214644945, -11.85413878919601771, 16.28571428571428470 ) ) ;
#7325 = CARTESIAN_POINT ( 'NONE',  ( -8.464561979789474222, -4.312909747525728754, 17.39999999999997016 ) ) ;
#7326 = CARTESIAN_POINT ( 'NONE',  ( -1.689666864740335228, 10.36326688006723273, 10.29886208192143293 ) ) ;
#7327 = VERTEX_POINT ( 'NONE', #1428 ) ;
#7328 = CARTESIAN_POINT ( 'NONE',  ( -4.742819248065502258, -13.55419868402813677, 22.07142857142858006 ) ) ;
#7329 = ORIENTED_EDGE ( 'NONE', *, *, #755, .T. ) ;
#7330 = FACE_OUTER_BOUND ( 'NONE', #7480, .T. ) ;
#7331 = VECTOR ( 'NONE', #1095, 999.9999999999998863 ) ;
#7332 = CARTESIAN_POINT ( 'NONE',  ( -8.731428362939187338, 13.89598863503036164, 12.21428571428571708 ) ) ;
#7333 = CARTESIAN_POINT ( 'NONE',  ( -5.297344310588352201, -15.53355953199867301, 42.06738800180214355 ) ) ;
#7334 = CARTESIAN_POINT ( 'NONE',  ( 5.012215536711511987, -9.837026868205997587, 7.649999999999992362 ) ) ;
#7335 = CARTESIAN_POINT ( 'NONE',  ( -1.727091770866549414, -10.90442828429184630, 13.95000000000002593 ) ) ;
#7336 = CARTESIAN_POINT ( 'NONE',  ( 4.623906867372411078, -13.21436662431711717, 9.428571428571425272 ) ) ;
#7337 = ADVANCED_FACE ( 'NONE', ( #5394, #9957 ), #5238, .T. ) ;
#7338 = CARTESIAN_POINT ( 'NONE',  ( 7.750357176954296712, -12.08964793087877787, 23.21024514465928235 ) ) ;
#7339 = ORIENTED_EDGE ( 'NONE', *, *, #3626, .T. ) ;
#7340 = CARTESIAN_POINT ( 'NONE',  ( -7.424621202458789426, 7.424621202458723701, 15.00000000000001421 ) ) ;
#7341 = LINE ( 'NONE', #57, #4854 ) ;
#7342 = CARTESIAN_POINT ( 'NONE',  ( -13.89774397934249706, -1.693770420379375974, 37.13881657323070584 ) ) ;
#7343 = CARTESIAN_POINT ( 'NONE',  ( -10.36326688006724162, 1.689666864740236640, 13.70113791807854398 ) ) ;
#7344 = CARTESIAN_POINT ( 'NONE',  ( 4.967534682030706250, -9.859792900771036983, 0.6511379180785785703 ) ) ;
#7345 = DIRECTION ( 'NONE',  ( 0.000000000000000000, -8.191099868251446680E-34, -1.000000000000000000 ) ) ;
#7346 = CARTESIAN_POINT ( 'NONE',  ( 13.17239914596754424, -4.743843029824685864, 18.57546914105500235 ) ) ;
#7347 = SHAPE_REPRESENTATION_RELATIONSHIP ( 'NONE' , 'NONE' ,  #4550, #2413 ) ;
#7348 = CARTESIAN_POINT ( 'NONE',  ( 4.865839792409144771, 13.51115193377589740, 23.07546914105501301 ) ) ;
#7349 = CARTESIAN_POINT ( 'NONE',  ( 7.806708723663831506, 7.806708723663925653, 9.749999999999982236 ) ) ;
#7350 = CARTESIAN_POINT ( 'NONE',  ( -2.000000000000001776, -9.511495879682425741E-17, 0.000000000000000000 ) ) ;
#7351 = CARTESIAN_POINT ( 'NONE',  ( -11.31370849898482156, 11.31370849898469544, 18.00000000000000355 ) ) ;
#7352 = CARTESIAN_POINT ( 'NONE',  ( 15.44746603149413922, 5.543385399275817527, 15.92453085894499409 ) ) ;
#7353 = DIRECTION ( 'NONE',  ( 1.000000000000000000, 0.000000000000000000, 0.000000000000000000 ) ) ;
#7354 = CARTESIAN_POINT ( 'NONE',  ( -167.1500000000000057, -0.2844360088669644626, 15.00000000000000000 ) ) ;
#7355 = CARTESIAN_POINT ( 'NONE',  ( -6.683790977649319842, 6.751237864895094809, 2.001137918078543354 ) ) ;
#7356 = CARTESIAN_POINT ( 'NONE',  ( -9.865911304835474738, -1.562606840307925626, 14.55000000000000249 ) ) ;
#7357 = DIRECTION ( 'NONE',  ( 0.000000000000000000, -8.191099868251446680E-34, -1.000000000000000000 ) ) ;
#7358 = CARTESIAN_POINT ( 'NONE',  ( 5.543385399275644332, 15.44746603149420494, 35.07546914105501656 ) ) ;
#7359 = CARTESIAN_POINT ( 'NONE',  ( 1.607813917173038121, -14.26974319298267346, 27.64285714285714590 ) ) ;
#7360 = CARTESIAN_POINT ( 'NONE',  ( 13.91197093850538380, 1.567502665446386390, 32.14285714285714590 ) ) ;
#7361 = ORIENTED_EDGE ( 'NONE', *, *, #433, .F. ) ;
#7362 = CARTESIAN_POINT ( 'NONE',  ( 11.31370849898482334, -11.31370849898469366, 27.00000000000000355 ) ) ;
#7363 = DIRECTION ( 'NONE',  ( 1.000000000000000000, 0.000000000000000000, 0.000000000000000000 ) ) ;
#7364 = CARTESIAN_POINT ( 'NONE',  ( 13.54758718765249803, 8.512513224245457977, 13.71428571428571352 ) ) ;
#7365 = DIRECTION ( 'NONE',  ( 0.9983709538884036894, -0.05705644952114250629, 5.938629746412706501E-18 ) ) ;
#7366 = CARTESIAN_POINT ( 'NONE',  ( 8.922933199037192509, -4.490180821391404287, 17.34886208192141765 ) ) ;
#7367 = CARTESIAN_POINT ( 'NONE',  ( -10.89658364409024749, -1.776620879821559917, 18.54886208192142405 ) ) ;
#7368 = CARTESIAN_POINT ( 'NONE',  ( -8.620103694221995738, -13.47998361472161299, 14.28975485534072298 ) ) ;
#7369 = CARTESIAN_POINT ( 'NONE',  ( 5.420364854932001819, 15.49051278174644430, 25.07142857142858361 ) ) ;
#7370 = CARTESIAN_POINT ( 'NONE',  ( -2.525158672622311418, 13.94875038000408374, 48.57768213684325787 ) ) ;
#7371 = CARTESIAN_POINT ( 'NONE',  ( -5.543385399275643444, -15.44746603149420494, 2.075469141055009015 ) ) ;
#7372 = CARTESIAN_POINT ( 'NONE',  ( 13.21436662431716869, -4.623906867372263640, 8.571428571428569398 ) ) ;
#7373 = CARTESIAN_POINT ( 'NONE',  ( 9.865911304835478290, 1.562606840307950273, 19.04999999999997939 ) ) ;
#7374 = CARTESIAN_POINT ( 'NONE',  ( 9.859792900771104485, -4.967534682030585458, 8.348862081921442524 ) ) ;
#7375 = EDGE_LOOP ( 'NONE', ( #9863, #1853, #4553, #4621 ) ) ;
#7376 = CARTESIAN_POINT ( 'NONE',  ( -1.607813917173034124, 14.26974319298267524, 18.64285714285715656 ) ) ;
#7377 = ORIENTED_EDGE ( 'NONE', *, *, #9711, .F. ) ;
#7378 =( GEOMETRIC_REPRESENTATION_CONTEXT ( 3 ) GLOBAL_UNCERTAINTY_ASSIGNED_CONTEXT ( ( #1743 ) ) GLOBAL_UNIT_ASSIGNED_CONTEXT ( ( #365, #2834, #415 ) ) REPRESENTATION_CONTEXT ( 'NONE', 'WORKASPACE' ) );
#7379 = CARTESIAN_POINT ( 'NONE',  ( -13.89598863503045933, 8.731428362939027465, 29.78571428571428825 ) ) ;
#7380 = CARTESIAN_POINT ( 'NONE',  ( 11.51250119794888249, 11.69682198916847682, 39.49595943037357415 ) ) ;
#7381 = CARTESIAN_POINT ( 'NONE',  ( 7.806708723663831506, 7.806708723663931870, 3.749999999999997335 ) ) ;
#7382 = CARTESIAN_POINT ( 'NONE',  ( 4.623906867372411078, -13.21436662431711717, 15.42857142857143060 ) ) ;
#7383 = CARTESIAN_POINT ( 'NONE',  ( -4.619798703721853528, -13.59724543428036725, 30.06738800180214355 ) ) ;
#7384 = STYLED_ITEM ( 'NONE', ( #5330 ), #568 ) ;
#7385 =( BOUNDED_SURFACE ( )  B_SPLINE_SURFACE ( 3, 2, ( 
 ( #3594, #2870, #2764, #6013, #8400, #6675, #8305, #8353, #9192, #5913, #1176, #1325, #5155, #9859, #7578, #10009, #2050, #7528, #5203, #4273, #8459, #2919, #4481, #1227, #1271, #7636, #6064, #555, #6631, #4377, #4430, #5965, #453, #9238, #2156, #6726, #9914, #7424, #3704, #352, #7476, #5302, #3500, #9143, #2820, #501, #9815, #2716, #3648, #5860, #6785, #1948, #9963, #5097, #8247, #4325, #10215, #2971, #8616, #30, #6268, #4686, #7741, #610, #3961, #9345, #5555, #4537, #7883, #2255, #6220, #9296, #7691, #2309, #660, #1384, #5455, #8666, #1588, #8560, #5508, #4735, #2210, #6319, #6121, #9452, #5356, #7002, #2357, #809, #7833, #1539, #5403, #1485, #7107, #10114, #6948, #3908, #3184, #9501, #8510, #2407, #7054, #3757, #6890, #713, #10059, #3028, #3811, #4636, #7794, #3862, #10162, #3076, #9397, #5602, #235, #3280, #914, #1785, #4210, #6474, #1738, #9654, #8714, #2656, #7362, #2606, #5657, #2559, #9698, #287, #6519, #864, #7210, #5703, #184, #9604, #3430, #6567, #7987, #2508, #1636, #5750, #4783, #1693, #1835, #8918, #3338, #8825, #4063, #3386, #7935, #4888, #9750, #128, #7311, #8871, #4937, #4014, #7161, #4990, #79, #8084, #3232, #8134, #1015, #4834, #6371, #9549, #6423, #2456, #8767, #8036, #963, #4165, #4113, #7259, #6713, #5848, #9998, #9897, #2855, #6000, #2752, #9951, #9179, #3487, #541, #337, #3631, #6617, #1210, #6766, #2085, #9130, #5951, #6665, #389, #5233, #4313, #1161, #2032, #7564, #8388, #9802, #1310, #2803, #4463, #7620, #8289, #3690, #3581, #6824, #9025, #7410, #5802, #7463, #4361, #8979, #7514, #1890, #5190, #439, #3539, #5141, #5038, #5897, #8338, #8184, #5083, #1256, #1117 ),
 ( #4415, #486, #4261, #2706, #1936, #8234, #9848, #751, #7729, #7091, #3013, #5441, #2906, #6256, #3741, #1369, #10201, #9283, #6157, #4724, #2140, #6876, #6105, #9224, #5284, #8444, #7870, #5345, #796, #2346, #595, #8498, #2958, #9436, #3898, #9333, #4521, #5496, #8655, #7041, #5389, #7679, #4622, #10046, #8549, #2297, #2197, #1424, #3946, #6931, #4674, #648, #3797, #10103, #1474, #7780, #703, #3850, #6988, #10151, #3064, #6208, #9383, #8601, #7824, #15, #2394, #3171, #6308, #9489, #5543, #3928, #1503, #3148, #5423, #827, #3206, #9520, #7757, #7902, #778, #630, #9364, #48, #7809, #6139, #7024, #3983, #3831, #5477, #4758, #8638, #733, #7132, #9416, #7072, #5526, #8530, #4656, #10182, #6288, #1607, #1456, #3047, #9315, #6340, #5739, #682, #3881, #2426, #5572, #2375, #8735, #10080, #8685, #8580, #6910, #4606, #6969, #4558, #7709, #3778, #3098, #2996, #2229, #5374, #10131, #6189, #2276, #6238, #2328, #1559, #4705, #7854, #9474, #2528, #6445, #5769, #149, #7229, #1803, #3404, #8944, #2472, #1857, #8891, #4229, #306, #4132, #2623, #9671, #5007, #4857, #3251, #8154, #3304, #208, #9772, #3358, #3447, #1039, #6493, #9625, #983, #1088, #8846, #2580, #6589, #934, #4183, #6540, #7284, #256, #5677, #9719, #7380, #4079, #1756, #5722, #2675, #4907, #8792, #5821, #8053, #4958, #8110, #1655, #7333, #4805, #7956, #886, #4036, #7181, #97, #6391, #9569, #5626, #1711, #8004, #1134, #7482, #6732, #461, #9866, #3710, #562, #8255, #2771, #1907, #6792, #5056, #1954, #2108, #9969, #3600, #5918, #1182, #3655, #2927, #9094, #6844, #410, #7584, #9923, #9149, #8202, #8998, #509, #360, #5971, #7642, #2877, #2056 ),
 ( #6682, #2826, #6637, #4279, #5209, #9044, #7431, #8359, #5161, #4331, #8312, #9821, #3507, #2723, #1232, #6019, #4383, #5251, #7534, #1280, #4438, #9198, #8407, #3554, #5866, #2007, #1334, #5103, #4488, #10015, #6070, #1391, #2165, #5309, #9245, #8466, #9889, #9122, #1975, #5888, #5133, #4567, #8331, #641, #5336, #3571, #1249, #5942, #2950, #6868, #5993, #4353, #6094, #9275, #10038, #9172, #430, #7612, #2792, #2078, #5274, #5182, #8280, #1417, #9943, #4514, #2189, #8491, #3790, #4455, #2024, #3620, #1202, #7505, #6705, #2848, #1303, #4406, #6757, #5226, #9067, #3682, #7555, #7671, #478, #587, #8437, #8380, #3732, #533, #7721, #6920, #10095, #6817, #9991, #2132, #2897, #6041, #9217, #1361, #4614, #8647, #1667, #2289, #3939, #3215, #7083, #9426, #9530, #5, #5536, #3996, #10142, #10194, #1570, #4765, #59, #3056, #1518, #7769, #4816, #8695, #5432, #2337, #7966, #896, #7141, #6150, #1465, #9326, #3890, #5382, #6200, #4665, #2236, #696, #7816, #3843, #3162, #7034, #4716, #6300, #1617, #4237, #8013, #5063, #4868, #8161, #945, #5732, #1096, #7388, #3412, #265, #7292, #4919, #315, #8854, #5684, #6548, #1867, #3456, #4091, #6598, #7342, #2685, #9004, #2587, #9783, #8119, #5828, #3315, #1722, #1915, #1764, #8899, #8211, #1813, #1141, #9731, #4970, #8064, #9680, #107, #215, #1049, #3260, #9634, #2632, #5015, #4193, #8954, #3366, #6402, #9578, #2538, #6500, #5780, #2483, #5637, #7240, #8804, #158, #6455, #522, #10030, #1290, #6741, #4446, #7442, #1405, #6083, #1349, #4394, #7597, #4504, #2940, #7658, #9831, #5929, #3670, #9160, #8322, #2182, #9260, #9877, #1240, #368, #576, #3518, #419, #3721, #5325 ),
 ( #9107, #2121, #6804, #9981, #6646, #2731, #8481, #9055, #5877, #5113, #8267, #1190, #3562, #4340, #7493, #5172, #9934, #2837, #5981, #2067, #8882, #1702, #7172, #8100, #7222, #89, #4028, #3244, #2668, #6434, #8989, #3440, #4847, #9617, #4073, #1081, #5000, #4123, #5616, #4223, #7372, #8146, #7272, #8784, #5712, #7997, #198, #3396, #3293, #6382, #9764, #8046, #2616, #299, #6580, #1900, #2571, #140, #1749, #9561, #925, #2519, #975, #9663, #5668, #4898, #3350, #8836, #1796, #6485, #5761, #1029, #8933, #6531, #4175, #1850, #7324, #5813, #5049, #8194, #247, #9710, #7577, #7422, #5912, #6835, #4376, #2715, #3593, #554, #404, #2049, #1324, #8352, #7527, #4480, #5964, #3647, #2099, #5096, #8304, #6725, #2868, #8399, #8246, #9858, #5859, #10008, #500, #7475, #1226, #7635, #3703, #9191, #2155, #6630, #5244, #2000, #3499, #1174, #3547, #2918, #351, #452, #6674, #9913, #1947, #9814, #9036, #2819, #6012, #1270, #6063, #4429, #6783, #9237, #5301, #1126, #9086, #4272, #4324, #2763, #5153, #608, #8458, #1383, #4536, #3756, #7690, #6764, #7360, #1887, #6710, #9747, #5139, #9949, #2799, #1208, #4258, #284, #484, #5846, #2083, #1066, #4413, #1934, #2750, #8977, #4208, #9072, #8182, #8132, #1981, #5188, #8336, #5080, #2030, #1254, #5036, #2853, #1115, #5949, #7408, #3537, #9128, #7561, #4359, #8287, #8232, #2704, #3627, #6615, #3484, #7512, #9895, #5998, #334, #9177, #437, #3428, #1158, #387, #4311, #5894, #7461, #6663, #9846, #3579, #593, #3795, #3114, #6928, #3896, #4620, #10101, #10044, #4572, #6206, #2195, #6155, #7039, #4519, #7777, #6986, #7727, #3848, #3739, #10149, #3062, #7677, #9281, #9331, #9381 ),
 ( #9996, #3011, #9222, #8496, #701, #6874, #1308, #749, #5343, #2295, #5438, #8599, #6254, #2242, #1367, #2956, #7618, #3688, #2904, #1422, #646, #5281, #6102, #5387, #8386, #8547, #539, #1524, #6822, #4672, #7822, #1471, #10199, #9433, #5231, #4460, #6048, #8442, #2138, #8812, #9535, #3267, #4149, #4770, #4874, #4099, #1675, #950, #846, #7245, #165, #7917, #6357, #6408, #3325, #4001, #2392, #6461, #7147, #64, #5643, #4924, #114, #5588, #9585, #2343, #6506, #998, #9640, #2442, #2492, #2546, #8071, #5690, #4722, #3220, #1728, #4049, #8750, #7298, #220, #4821, #7972, #5495, #1771, #8653, #5541, #3373, #1575, #7196, #901, #8019, #7868, #794, #3944, #7089, #12, #3168, #6306, #8701, #8905, #2593, #8274, #1056, #6651, #8472, #4345, #2737, #8962, #1819, #2173, #7396, #3770, #4976, #6075, #3465, #4294, #7348, #4198, #375, #9736, #271, #3526, #6850, #10021, #2692, #2933, #9251, #3417, #622, #6553, #7499, #5022, #5068, #5315, #8166, #9061, #1969, #5834, #4244, #1102, #9011, #1920, #5121, #1195, #8219, #671, #818, #3917, #9512, #5566, #9406, #7893, #4697, #39, #10122, #1447, #7123, #2266, #5468, #4795, #1550, #8727, #9464, #7844, #7802, #770, #3197, #6903, #876, #1648, #6332, #3872, #7062, #2418, #7948, #4748, #9307, #5413, #10225, #3135, #724, #10070, #2220, #6179, #7015, #5366, #6960, #3039, #9356, #10172, #3087, #2366, #5518, #1599, #7265, #6526, #6378, #4171, #871, #971, #3288, #2515, #1594, #2362, #4120, #3968, #9613, #1023, #194, #5664, #8722, #4744, #4944, #85, #5515, #8675, #8879, #3240, #7217, #35, #7890, #6429, #2415, #815, #8832, #9659, #2567, #9557, #6480, #5708, #3192, #7320 ),
 ( #1744, #2462, #7167, #1792, #4023, #7943, #4894, #3346, #8092, #6328, #243, #8042, #3392, #7119, #4843, #9509, #136, #5561, #1644, #4788, #5610, #8780, #921, #1698, #4069, #7993, #9081, #1168, #4268, #9031, #447, #6624, #399, #1266, #8985, #1992, #1221, #1942, #8299, #8190, #4372, #7524, #1896, #3495, #3544, #3589, #7417, #6575, #6722, #344, #5045, #2758, #2043, #7470, #2711, #6671, #9907, #9854, #5906, #8925, #9705, #2814, #1077, #5149, #8349, #5960, #9139, #5809, #1845, #5199, #9810, #3641, #2612, #4425, #5855, #4321, #7368, #5757, #7574, #9757, #4996, #496, #8142, #4217, #5092, #294, #3437, #2664, #8241, #551, #7790, #3698, #4582, #10159, #2305, #3024, #6942, #3750, #1380, #8612, #5296, #2149, #5399, #1536, #759, #6832, #6779, #2864, #9188, #2914, #9293, #9233, #10056, #6115, #7099, #5505, #4109, #9497, #2451, #1780, #5597, #2555, #3276, #8760, #8710, #6366, #4884, #858, #4830, #5699, #2403, #6417, #5652, #9544, #2503, #5551, #8821, #8029, #1632, #7929, #7983, #959, #4010, #3954, #7254, #7157, #1688, #7205, #4933, #910, #4059, #124, #7050, #10211, #3123, #176, #9596, #3334, #6263, #9448, #2354, #8663, #1585, #4732, #7879, #5034, #5946, #2797, #281, #8179, #4158, #8284, #229, #7358, #4357, #7510, #5844, #7406, #3426, #435, #1009, #332, #9126, #2651, #3480, #9844, #6612, #3575, #9022, #8230, #7458, #2028, #3382, #8975, #6515, #2602, #4985, #7559, #1469, #537, #6761, #4618, #3686, #7675, #6984, #482, #2901, #6046, #2136, #591, #3736, #10147, #6872, #3060, #7775, #10042, #2954, #6100, #6204, #2240, #9279, #2193, #9379, #2293, #5340, #6926, #10099, #4669, #8597, #1522, #7820, #747, #5436 ),
 ( #1393, #2983, #7644, #6846, #2929, #2217, #668, #8468, #5363, #8519, #8409, #3035, #564, #3867, #6072, #7010, #721, #1443, #10168, #3821, #1546, #3913, #10221, #4546, #8625, #5464, #1336, #6956, #7059, #9352, #9247, #2262, #7840, #7699, #5410, #6277, #8568, #9460, #5253, #4490, #2167, #618, #3765, #6899, #5580, #4865, #9632, #7081, #1615, #4714, #4915, #6400, #6298, #7139, #8062, #990, #4088, #10192, #5488, #3107, #56, #1568, #2, #9482, #6247, #787, #6350, #2385, #9528, #3159, #7910, #8743, #7964, #4043, #7189, #2481, #5635, #9728, #3364, #9678, #4191, #6546, #5838, #8278, #7351, #5938, #1879, #5027, #2790, #8172, #9015, #4403, #1106, #4249, #323, #2696, #1924, #5072, #476, #8223, #3618, #6753, #1150, #4298, #7453, #9118, #6701, #3530, #9839, #5886, #9065, #9887, #1973, #5126, #1200, #4350, #7503, #427, #2130, #9170, #8590, #6865, #7767, #6979, #10140, #742, #1415, #5272, #584, #3680, #6813, #8432, #9271, #8489, #7668, #3730, #4565, #5990, #638, #7718, #693, #6918, #3841, #8539, #3004, #3054, #6147, #2285, #1515, #2076, #6198, #5430, #6346, #5483, #5530, #1564, #9524, #1612, #783, #3934, #7078, #7877, #2401, #804, #1583, #1533, #3179, #10209, #3121, #25, #4918, #8803, #1721, #4867, #6454, #944, #4090, #7239, #4949, #8099, #8932, #8876, #241, #8139, #2002, #454, #1228, #2102, #9193, #9915, #3595, #2920, #7529, #4378, #5246, #556, #6065, #9860, #9239, #6014, #5156, #6727, #2821, #8401, #1326, #5966, #9144, #2157, #2051, #5204, #4482, #3705, #5303, #2765, #8460, #7637, #1385, #7692, #1272, #10010, #6786, #4538, #8306, #406, #611, #8354, #7579, #6891, #502, #3758, #6838, #3649, #4431 ) ),
 .UNSPECIFIED., .T., .F., .F. ) 
 B_SPLINE_SURFACE_WITH_KNOTS ( ( 4, 3, 4 ),
 ( 3, 2, 2, 2, 2, 2, 2, 2, 2, 2, 2, 2, 2, 2, 2, 2, 2, 2, 2, 2, 2, 2, 2, 2, 2, 2, 2, 2, 2, 2, 2, 2, 2, 2, 2, 2, 2, 2, 2, 2, 2, 2, 2, 2, 2, 2, 2, 2, 2, 2, 2, 2, 2, 2, 2, 2, 2, 2, 2, 2, 2, 2, 2, 2, 2, 2, 2, 2, 2, 2, 2, 2, 2, 2, 2, 2, 2, 2, 2, 2, 2, 2, 2, 2, 2, 2, 2, 2, 2, 2, 2, 2, 2, 2, 2, 2, 2, 2, 2, 2, 2, 2, 2, 2, 2, 2, 2, 2, 2, 2, 2, 2, 2, 2, 2, 2, 3 ),
 ( 0.000000000000000000, 0.5000000000000000000, 1.000000000000000000 ),
 ( 0.000000000000000000, 0.007936507936507936067, 0.01587301587301587213, 0.02380952380952380820, 0.03174603174603174427, 0.03968253968253968034, 0.04761904761904761640, 0.05555555555555555247, 0.06349206349206348854, 0.07142857142857142461, 0.07936507936507936067, 0.08730158730158729674, 0.09523809523809523281, 0.1031746031746031689, 0.1111111111111111049, 0.1190476190476190410, 0.1269841269841269771, 0.1349206349206349131, 0.1428571428571428492, 0.1507936507936507853, 0.1587301587301587213, 0.1666666666666666574, 0.1746031746031745935, 0.1825396825396825295, 0.1904761904761904656, 0.1984126984126984017, 0.2063492063492063378, 0.2142857142857142738, 0.2222222222222222099, 0.2301587301587301460, 0.2380952380952380820, 0.2460317460317460181, 0.2539682539682539542, 0.2619047619047619180, 0.2698412698412698263, 0.2777777777777777901, 0.2857142857142856984, 0.2936507936507936622, 0.3015873015873015706, 0.3095238095238095344, 0.3174603174603174427, 0.3253968253968254065, 0.3333333333333333148, 0.3412698412698412787, 0.3492063492063491870, 0.3571428571428571508, 0.3650793650793650591, 0.3730158730158730229, 0.3809523809523809312, 0.3888888888888888951, 0.3968253968253968034, 0.4047619047619047672, 0.4126984126984126755, 0.4206349206349206393, 0.4285714285714285476, 0.4365079365079365115, 0.4444444444444444198, 0.4523809523809523836, 0.4603174603174602919, 0.4682539682539682557, 0.4761904761904761640, 0.4841269841269841279, 0.4920634920634920362, 0.5000000000000000000, 0.5079365079365079083, 0.5158730158730159276, 0.5238095238095238360, 0.5317460317460317443, 0.5396825396825396526, 0.5476190476190476719, 0.5555555555555555802, 0.5634920634920634885, 0.5714285714285713969, 0.5793650793650794162, 0.5873015873015873245, 0.5952380952380952328, 0.6031746031746031411, 0.6111111111111111605, 0.6190476190476190688, 0.6269841269841269771, 0.6349206349206348854, 0.6428571428571429047, 0.6507936507936508130, 0.6587301587301587213, 0.6666666666666666297, 0.6746031746031746490, 0.6825396825396825573, 0.6904761904761904656, 0.6984126984126983739, 0.7063492063492063933, 0.7142857142857143016, 0.7222222222222222099, 0.7301587301587301182, 0.7380952380952381375, 0.7460317460317460458, 0.7539682539682539542, 0.7619047619047618625, 0.7698412698412698818, 0.7777777777777777901, 0.7857142857142856984, 0.7936507936507936067, 0.8015873015873016261, 0.8095238095238095344, 0.8174603174603174427, 0.8253968253968253510, 0.8333333333333333703, 0.8412698412698412787, 0.8492063492063491870, 0.8571428571428570953, 0.8650793650793651146, 0.8730158730158730229, 0.8809523809523809312, 0.8888888888888888395, 0.8968253968253968589, 0.9047619047619047672, 0.9126984126984126755, 0.9166666666666666297 ),
 .UNSPECIFIED. ) 
 GEOMETRIC_REPRESENTATION_ITEM ( )  RATIONAL_B_SPLINE_SURFACE ( (
 ( 1.000000000000000000, 0.9749279121818236193, 1.000000000000000000, 0.9749279121818236193, 1.000000000000000000, 0.9749279121818236193, 1.000000000000000000, 0.9749279121818236193, 1.000000000000000000, 0.9749279121818236193, 1.000000000000000000, 0.9749279121818236193, 1.000000000000000000, 0.9749279121818236193, 1.000000000000000000, 0.9749279121818236193, 1.000000000000000000, 0.9749279121818236193, 1.000000000000000000, 0.9749279121818236193, 1.000000000000000000, 0.9749279121818236193, 1.000000000000000000, 0.9749279121818236193, 1.000000000000000000, 0.9749279121818236193, 1.000000000000000000, 0.9749279121818236193, 1.000000000000000000, 0.9749279121818236193, 1.000000000000000000, 0.9749279121818236193, 1.000000000000000000, 0.9749279121818236193, 1.000000000000000000, 0.9749279121818236193, 1.000000000000000000, 0.9749279121818236193, 1.000000000000000000, 0.9749279121818236193, 1.000000000000000000, 0.9749279121818236193, 1.000000000000000000, 0.9749279121818236193, 1.000000000000000000, 0.9749279121818236193, 1.000000000000000000, 0.9749279121818236193, 1.000000000000000000, 0.9749279121818236193, 1.000000000000000000, 0.9749279121818236193, 1.000000000000000000, 0.9749279121818236193, 1.000000000000000000, 0.9749279121818236193, 1.000000000000000000, 0.9749279121818236193, 1.000000000000000000, 0.9749279121818236193, 1.000000000000000000, 0.9749279121818236193, 1.000000000000000000, 0.9749279121818236193, 1.000000000000000000, 0.9749279121818236193, 1.000000000000000000, 0.9749279121818236193, 1.000000000000000000, 0.9749279121818236193, 1.000000000000000000, 0.9749279121818236193, 1.000000000000000000, 0.9749279121818236193, 1.000000000000000000, 0.9749279121818236193, 1.000000000000000000, 0.9749279121818236193, 1.000000000000000000, 0.9749279121818236193, 1.000000000000000000, 0.9749279121818236193, 1.000000000000000000, 0.9749279121818236193, 1.000000000000000000, 0.9749279121818236193, 1.000000000000000000, 0.9749279121818236193, 1.000000000000000000, 0.9749279121818236193, 1.000000000000000000, 0.9749279121818236193, 1.000000000000000000, 0.9749279121818236193, 1.000000000000000000, 0.9749279121818236193, 1.000000000000000000, 0.9749279121818236193, 1.000000000000000000, 0.9749279121818236193, 1.000000000000000000, 0.9749279121818236193, 1.000000000000000000, 0.9749279121818236193, 1.000000000000000000, 0.9749279121818236193, 1.000000000000000000, 0.9749279121818236193, 1.000000000000000000, 0.9749279121818236193, 1.000000000000000000, 0.9749279121818236193, 1.000000000000000000, 0.9749279121818236193, 1.000000000000000000, 0.9749279121818236193, 1.000000000000000000, 0.9749279121818236193, 1.000000000000000000, 0.9749279121818236193, 1.000000000000000000, 0.9749279121818236193, 1.000000000000000000, 0.9749279121818236193, 1.000000000000000000, 0.9749279121818236193, 1.000000000000000000, 0.9749279121818236193, 1.000000000000000000, 0.9749279121818236193, 1.000000000000000000, 0.9749279121818236193, 1.000000000000000000, 0.9749279121818236193, 1.000000000000000000, 0.9749279121818236193, 1.000000000000000000, 0.9749279121818236193, 1.000000000000000000, 0.9749279121818236193, 1.000000000000000000, 0.9749279121818236193, 1.000000000000000000, 0.9749279121818236193, 1.000000000000000000, 0.9749279121818236193, 1.000000000000000000, 0.9749279121818236193, 1.000000000000000000, 0.9749279121818236193, 1.000000000000000000, 0.9749279121818236193, 1.000000000000000000, 0.9749279121818236193, 1.000000000000000000, 0.9749279121818236193, 1.000000000000000000, 0.9749279121818236193, 1.000000000000000000, 0.9749279121818236193, 1.000000000000000000, 0.9749279121818236193, 1.000000000000000000, 0.9749279121818236193, 1.000000000000000000, 0.9749279121818236193, 1.000000000000000000, 0.9749279121818236193, 1.000000000000000000, 0.9749279121818236193, 1.000000000000000000, 0.9749279121818236193, 1.000000000000000000, 0.9749279121818236193, 1.000000000000000000, 0.9749279121818236193, 1.000000000000000000, 0.9749279121818236193, 1.000000000000000000, 0.9749279121818236193, 1.000000000000000000, 0.9749279121818236193, 1.000000000000000000, 0.9749279121818236193, 1.000000000000000000, 0.9749279121818236193, 1.000000000000000000, 0.9749279121818236193, 1.000000000000000000, 0.9749279121818236193, 1.000000000000000000, 0.9749279121818236193, 1.000000000000000000, 0.9749279121818236193, 1.000000000000000000, 0.9749279121818236193, 1.000000000000000000, 0.9749279121818236193, 1.000000000000000000, 0.9749279121818236193, 1.000000000000000000, 0.9749279121818236193, 1.000000000000000000, 0.9749279121818236193, 1.000000000000000000, 0.9749279121818236193, 1.000000000000000000, 0.9749279121818236193, 1.000000000000000000, 0.9749279121818236193, 1.000000000000000000, 0.9749279121818236193, 1.000000000000000000, 0.9749279121818236193, 1.000000000000000000, 0.9749279121818236193, 1.000000000000000000, 0.9749279121818236193, 1.000000000000000000, 0.9749279121818236193, 1.000000000000000000, 0.9749279121818236193, 1.000000000000000000, 0.9749279121818236193, 1.000000000000000000, 0.9749279121818236193, 1.000000000000000000, 0.9749279121818236193, 1.000000000000000000, 0.9749279121818236193, 1.000000000000000000, 0.9874639560909117542, 0.9874639560909117542),
 ( 0.3333333333333333703, 0.3249759707272745768, 0.3333333333333333703, 0.3249759707272745768, 0.3333333333333333703, 0.3249759707272745768, 0.3333333333333333703, 0.3249759707272745768, 0.3333333333333333703, 0.3249759707272745768, 0.3333333333333333703, 0.3249759707272745768, 0.3333333333333333703, 0.3249759707272745768, 0.3333333333333333703, 0.3249759707272745768, 0.3333333333333333703, 0.3249759707272745768, 0.3333333333333333703, 0.3249759707272745768, 0.3333333333333333703, 0.3249759707272745768, 0.3333333333333333703, 0.3249759707272745768, 0.3333333333333333703, 0.3249759707272745768, 0.3333333333333333703, 0.3249759707272745768, 0.3333333333333333703, 0.3249759707272745768, 0.3333333333333333703, 0.3249759707272745768, 0.3333333333333333703, 0.3249759707272745768, 0.3333333333333333703, 0.3249759707272745768, 0.3333333333333333703, 0.3249759707272745768, 0.3333333333333333703, 0.3249759707272745768, 0.3333333333333333703, 0.3249759707272745768, 0.3333333333333333703, 0.3249759707272745768, 0.3333333333333333703, 0.3249759707272745768, 0.3333333333333333703, 0.3249759707272745768, 0.3333333333333333703, 0.3249759707272745768, 0.3333333333333333703, 0.3249759707272745768, 0.3333333333333333703, 0.3249759707272745768, 0.3333333333333333703, 0.3249759707272745768, 0.3333333333333333703, 0.3249759707272745768, 0.3333333333333333703, 0.3249759707272745768, 0.3333333333333333703, 0.3249759707272745768, 0.3333333333333333703, 0.3249759707272745768, 0.3333333333333333703, 0.3249759707272745768, 0.3333333333333333703, 0.3249759707272745768, 0.3333333333333333703, 0.3249759707272745768, 0.3333333333333333703, 0.3249759707272745768, 0.3333333333333333703, 0.3249759707272745768, 0.3333333333333333703, 0.3249759707272745768, 0.3333333333333333703, 0.3249759707272745768, 0.3333333333333333703, 0.3249759707272745768, 0.3333333333333333703, 0.3249759707272745768, 0.3333333333333333703, 0.3249759707272745768, 0.3333333333333333703, 0.3249759707272745768, 0.3333333333333333703, 0.3249759707272745768, 0.3333333333333333703, 0.3249759707272745768, 0.3333333333333333703, 0.3249759707272745768, 0.3333333333333333703, 0.3249759707272745768, 0.3333333333333333703, 0.3249759707272745768, 0.3333333333333333703, 0.3249759707272745768, 0.3333333333333333703, 0.3249759707272745768, 0.3333333333333333703, 0.3249759707272745768, 0.3333333333333333703, 0.3249759707272745768, 0.3333333333333333703, 0.3249759707272745768, 0.3333333333333333703, 0.3249759707272745768, 0.3333333333333333703, 0.3249759707272745768, 0.3333333333333333703, 0.3249759707272745768, 0.3333333333333333703, 0.3249759707272745768, 0.3333333333333333703, 0.3249759707272745768, 0.3333333333333333703, 0.3249759707272745768, 0.3333333333333333703, 0.3249759707272745768, 0.3333333333333333703, 0.3249759707272745768, 0.3333333333333333703, 0.3249759707272745768, 0.3333333333333333703, 0.3249759707272745768, 0.3333333333333333703, 0.3249759707272745768, 0.3333333333333333703, 0.3249759707272745768, 0.3333333333333333703, 0.3249759707272745768, 0.3333333333333333703, 0.3249759707272745768, 0.3333333333333333703, 0.3249759707272745768, 0.3333333333333333703, 0.3249759707272745768, 0.3333333333333333703, 0.3249759707272745768, 0.3333333333333333703, 0.3249759707272745768, 0.3333333333333333703, 0.3249759707272745768, 0.3333333333333333703, 0.3249759707272745768, 0.3333333333333333703, 0.3249759707272745768, 0.3333333333333333703, 0.3249759707272745768, 0.3333333333333333703, 0.3249759707272745768, 0.3333333333333333703, 0.3249759707272745768, 0.3333333333333333703, 0.3249759707272745768, 0.3333333333333333703, 0.3249759707272745768, 0.3333333333333333703, 0.3249759707272745768, 0.3333333333333333703, 0.3249759707272745768, 0.3333333333333333703, 0.3249759707272745768, 0.3333333333333333703, 0.3249759707272745768, 0.3333333333333333703, 0.3249759707272745768, 0.3333333333333333703, 0.3249759707272745768, 0.3333333333333333703, 0.3249759707272745768, 0.3333333333333333703, 0.3249759707272745768, 0.3333333333333333703, 0.3249759707272745768, 0.3333333333333333703, 0.3249759707272745768, 0.3333333333333333703, 0.3249759707272745768, 0.3333333333333333703, 0.3249759707272745768, 0.3333333333333333703, 0.3249759707272745768, 0.3333333333333333703, 0.3249759707272745768, 0.3333333333333333703, 0.3249759707272745768, 0.3333333333333333703, 0.3249759707272745768, 0.3333333333333333703, 0.3249759707272745768, 0.3333333333333333703, 0.3249759707272745768, 0.3333333333333333703, 0.3249759707272745768, 0.3333333333333333703, 0.3249759707272745768, 0.3333333333333333703, 0.3249759707272745768, 0.3333333333333333703, 0.3249759707272745768, 0.3333333333333333703, 0.3249759707272745768, 0.3333333333333333703, 0.3249759707272745768, 0.3333333333333333703, 0.3249759707272745768, 0.3333333333333333703, 0.3249759707272745768, 0.3333333333333333703, 0.3249759707272745768, 0.3333333333333333703, 0.3249759707272745768, 0.3333333333333333703, 0.3249759707272745768, 0.3333333333333333703, 0.3249759707272745768, 0.3333333333333333703, 0.3249759707272745768, 0.3333333333333333703, 0.3249759707272745768, 0.3333333333333333703, 0.3249759707272745768, 0.3333333333333333703, 0.3249759707272745768, 0.3333333333333333703, 0.3249759707272745768, 0.3333333333333333703, 0.3249759707272745768, 0.3333333333333333703, 0.3291546520303039736, 0.3291546520303039736),
 ( 0.3333333333333333703, 0.3249759707272745768, 0.3333333333333333703, 0.3249759707272745768, 0.3333333333333333703, 0.3249759707272745768, 0.3333333333333333703, 0.3249759707272745768, 0.3333333333333333703, 0.3249759707272745768, 0.3333333333333333703, 0.3249759707272745768, 0.3333333333333333703, 0.3249759707272745768, 0.3333333333333333703, 0.3249759707272745768, 0.3333333333333333703, 0.3249759707272745768, 0.3333333333333333703, 0.3249759707272745768, 0.3333333333333333703, 0.3249759707272745768, 0.3333333333333333703, 0.3249759707272745768, 0.3333333333333333703, 0.3249759707272745768, 0.3333333333333333703, 0.3249759707272745768, 0.3333333333333333703, 0.3249759707272745768, 0.3333333333333333703, 0.3249759707272745768, 0.3333333333333333703, 0.3249759707272745768, 0.3333333333333333703, 0.3249759707272745768, 0.3333333333333333703, 0.3249759707272745768, 0.3333333333333333703, 0.3249759707272745768, 0.3333333333333333703, 0.3249759707272745768, 0.3333333333333333703, 0.3249759707272745768, 0.3333333333333333703, 0.3249759707272745768, 0.3333333333333333703, 0.3249759707272745768, 0.3333333333333333703, 0.3249759707272745768, 0.3333333333333333703, 0.3249759707272745768, 0.3333333333333333703, 0.3249759707272745768, 0.3333333333333333703, 0.3249759707272745768, 0.3333333333333333703, 0.3249759707272745768, 0.3333333333333333703, 0.3249759707272745768, 0.3333333333333333703, 0.3249759707272745768, 0.3333333333333333703, 0.3249759707272745768, 0.3333333333333333703, 0.3249759707272745768, 0.3333333333333333703, 0.3249759707272745768, 0.3333333333333333703, 0.3249759707272745768, 0.3333333333333333703, 0.3249759707272745768, 0.3333333333333333703, 0.3249759707272745768, 0.3333333333333333703, 0.3249759707272745768, 0.3333333333333333703, 0.3249759707272745768, 0.3333333333333333703, 0.3249759707272745768, 0.3333333333333333703, 0.3249759707272745768, 0.3333333333333333703, 0.3249759707272745768, 0.3333333333333333703, 0.3249759707272745768, 0.3333333333333333703, 0.3249759707272745768, 0.3333333333333333703, 0.3249759707272745768, 0.3333333333333333703, 0.3249759707272745768, 0.3333333333333333703, 0.3249759707272745768, 0.3333333333333333703, 0.3249759707272745768, 0.3333333333333333703, 0.3249759707272745768, 0.3333333333333333703, 0.3249759707272745768, 0.3333333333333333703, 0.3249759707272745768, 0.3333333333333333703, 0.3249759707272745768, 0.3333333333333333703, 0.3249759707272745768, 0.3333333333333333703, 0.3249759707272745768, 0.3333333333333333703, 0.3249759707272745768, 0.3333333333333333703, 0.3249759707272745768, 0.3333333333333333703, 0.3249759707272745768, 0.3333333333333333703, 0.3249759707272745768, 0.3333333333333333703, 0.3249759707272745768, 0.3333333333333333703, 0.3249759707272745768, 0.3333333333333333703, 0.3249759707272745768, 0.3333333333333333703, 0.3249759707272745768, 0.3333333333333333703, 0.3249759707272745768, 0.3333333333333333703, 0.3249759707272745768, 0.3333333333333333703, 0.3249759707272745768, 0.3333333333333333703, 0.3249759707272745768, 0.3333333333333333703, 0.3249759707272745768, 0.3333333333333333703, 0.3249759707272745768, 0.3333333333333333703, 0.3249759707272745768, 0.3333333333333333703, 0.3249759707272745768, 0.3333333333333333703, 0.3249759707272745768, 0.3333333333333333703, 0.3249759707272745768, 0.3333333333333333703, 0.3249759707272745768, 0.3333333333333333703, 0.3249759707272745768, 0.3333333333333333703, 0.3249759707272745768, 0.3333333333333333703, 0.3249759707272745768, 0.3333333333333333703, 0.3249759707272745768, 0.3333333333333333703, 0.3249759707272745768, 0.3333333333333333703, 0.3249759707272745768, 0.3333333333333333703, 0.3249759707272745768, 0.3333333333333333703, 0.3249759707272745768, 0.3333333333333333703, 0.3249759707272745768, 0.3333333333333333703, 0.3249759707272745768, 0.3333333333333333703, 0.3249759707272745768, 0.3333333333333333703, 0.3249759707272745768, 0.3333333333333333703, 0.3249759707272745768, 0.3333333333333333703, 0.3249759707272745768, 0.3333333333333333703, 0.3249759707272745768, 0.3333333333333333703, 0.3249759707272745768, 0.3333333333333333703, 0.3249759707272745768, 0.3333333333333333703, 0.3249759707272745768, 0.3333333333333333703, 0.3249759707272745768, 0.3333333333333333703, 0.3249759707272745768, 0.3333333333333333703, 0.3249759707272745768, 0.3333333333333333703, 0.3249759707272745768, 0.3333333333333333703, 0.3249759707272745768, 0.3333333333333333703, 0.3249759707272745768, 0.3333333333333333703, 0.3249759707272745768, 0.3333333333333333703, 0.3249759707272745768, 0.3333333333333333703, 0.3249759707272745768, 0.3333333333333333703, 0.3249759707272745768, 0.3333333333333333703, 0.3249759707272745768, 0.3333333333333333703, 0.3249759707272745768, 0.3333333333333333703, 0.3249759707272745768, 0.3333333333333333703, 0.3249759707272745768, 0.3333333333333333703, 0.3249759707272745768, 0.3333333333333333703, 0.3249759707272745768, 0.3333333333333333703, 0.3249759707272745768, 0.3333333333333333703, 0.3249759707272745768, 0.3333333333333333703, 0.3249759707272745768, 0.3333333333333333703, 0.3249759707272745768, 0.3333333333333333703, 0.3249759707272745768, 0.3333333333333333703, 0.3249759707272745768, 0.3333333333333333703, 0.3249759707272745768, 0.3333333333333333703, 0.3249759707272745768, 0.3333333333333333703, 0.3291546520303039736, 0.3291546520303039736),
 ( 1.000000000000000000, 0.9749279121818236193, 1.000000000000000000, 0.9749279121818236193, 1.000000000000000000, 0.9749279121818236193, 1.000000000000000000, 0.9749279121818236193, 1.000000000000000000, 0.9749279121818236193, 1.000000000000000000, 0.9749279121818236193, 1.000000000000000000, 0.9749279121818236193, 1.000000000000000000, 0.9749279121818236193, 1.000000000000000000, 0.9749279121818236193, 1.000000000000000000, 0.9749279121818236193, 1.000000000000000000, 0.9749279121818236193, 1.000000000000000000, 0.9749279121818236193, 1.000000000000000000, 0.9749279121818236193, 1.000000000000000000, 0.9749279121818236193, 1.000000000000000000, 0.9749279121818236193, 1.000000000000000000, 0.9749279121818236193, 1.000000000000000000, 0.9749279121818236193, 1.000000000000000000, 0.9749279121818236193, 1.000000000000000000, 0.9749279121818236193, 1.000000000000000000, 0.9749279121818236193, 1.000000000000000000, 0.9749279121818236193, 1.000000000000000000, 0.9749279121818236193, 1.000000000000000000, 0.9749279121818236193, 1.000000000000000000, 0.9749279121818236193, 1.000000000000000000, 0.9749279121818236193, 1.000000000000000000, 0.9749279121818236193, 1.000000000000000000, 0.9749279121818236193, 1.000000000000000000, 0.9749279121818236193, 1.000000000000000000, 0.9749279121818236193, 1.000000000000000000, 0.9749279121818236193, 1.000000000000000000, 0.9749279121818236193, 1.000000000000000000, 0.9749279121818236193, 1.000000000000000000, 0.9749279121818236193, 1.000000000000000000, 0.9749279121818236193, 1.000000000000000000, 0.9749279121818236193, 1.000000000000000000, 0.9749279121818236193, 1.000000000000000000, 0.9749279121818236193, 1.000000000000000000, 0.9749279121818236193, 1.000000000000000000, 0.9749279121818236193, 1.000000000000000000, 0.9749279121818236193, 1.000000000000000000, 0.9749279121818236193, 1.000000000000000000, 0.9749279121818236193, 1.000000000000000000, 0.9749279121818236193, 1.000000000000000000, 0.9749279121818236193, 1.000000000000000000, 0.9749279121818236193, 1.000000000000000000, 0.9749279121818236193, 1.000000000000000000, 0.9749279121818236193, 1.000000000000000000, 0.9749279121818236193, 1.000000000000000000, 0.9749279121818236193, 1.000000000000000000, 0.9749279121818236193, 1.000000000000000000, 0.9749279121818236193, 1.000000000000000000, 0.9749279121818236193, 1.000000000000000000, 0.9749279121818236193, 1.000000000000000000, 0.9749279121818236193, 1.000000000000000000, 0.9749279121818236193, 1.000000000000000000, 0.9749279121818236193, 1.000000000000000000, 0.9749279121818236193, 1.000000000000000000, 0.9749279121818236193, 1.000000000000000000, 0.9749279121818236193, 1.000000000000000000, 0.9749279121818236193, 1.000000000000000000, 0.9749279121818236193, 1.000000000000000000, 0.9749279121818236193, 1.000000000000000000, 0.9749279121818236193, 1.000000000000000000, 0.9749279121818236193, 1.000000000000000000, 0.9749279121818236193, 1.000000000000000000, 0.9749279121818236193, 1.000000000000000000, 0.9749279121818236193, 1.000000000000000000, 0.9749279121818236193, 1.000000000000000000, 0.9749279121818236193, 1.000000000000000000, 0.9749279121818236193, 1.000000000000000000, 0.9749279121818236193, 1.000000000000000000, 0.9749279121818236193, 1.000000000000000000, 0.9749279121818236193, 1.000000000000000000, 0.9749279121818236193, 1.000000000000000000, 0.9749279121818236193, 1.000000000000000000, 0.9749279121818236193, 1.000000000000000000, 0.9749279121818236193, 1.000000000000000000, 0.9749279121818236193, 1.000000000000000000, 0.9749279121818236193, 1.000000000000000000, 0.9749279121818236193, 1.000000000000000000, 0.9749279121818236193, 1.000000000000000000, 0.9749279121818236193, 1.000000000000000000, 0.9749279121818236193, 1.000000000000000000, 0.9749279121818236193, 1.000000000000000000, 0.9749279121818236193, 1.000000000000000000, 0.9749279121818236193, 1.000000000000000000, 0.9749279121818236193, 1.000000000000000000, 0.9749279121818236193, 1.000000000000000000, 0.9749279121818236193, 1.000000000000000000, 0.9749279121818236193, 1.000000000000000000, 0.9749279121818236193, 1.000000000000000000, 0.9749279121818236193, 1.000000000000000000, 0.9749279121818236193, 1.000000000000000000, 0.9749279121818236193, 1.000000000000000000, 0.9749279121818236193, 1.000000000000000000, 0.9749279121818236193, 1.000000000000000000, 0.9749279121818236193, 1.000000000000000000, 0.9749279121818236193, 1.000000000000000000, 0.9749279121818236193, 1.000000000000000000, 0.9749279121818236193, 1.000000000000000000, 0.9749279121818236193, 1.000000000000000000, 0.9749279121818236193, 1.000000000000000000, 0.9749279121818236193, 1.000000000000000000, 0.9749279121818236193, 1.000000000000000000, 0.9749279121818236193, 1.000000000000000000, 0.9749279121818236193, 1.000000000000000000, 0.9749279121818236193, 1.000000000000000000, 0.9749279121818236193, 1.000000000000000000, 0.9749279121818236193, 1.000000000000000000, 0.9749279121818236193, 1.000000000000000000, 0.9749279121818236193, 1.000000000000000000, 0.9749279121818236193, 1.000000000000000000, 0.9749279121818236193, 1.000000000000000000, 0.9749279121818236193, 1.000000000000000000, 0.9749279121818236193, 1.000000000000000000, 0.9874639560909117542, 0.9874639560909117542),
 ( 0.3333333333333333703, 0.3249759707272745768, 0.3333333333333333703, 0.3249759707272745768, 0.3333333333333333703, 0.3249759707272745768, 0.3333333333333333703, 0.3249759707272745768, 0.3333333333333333703, 0.3249759707272745768, 0.3333333333333333703, 0.3249759707272745768, 0.3333333333333333703, 0.3249759707272745768, 0.3333333333333333703, 0.3249759707272745768, 0.3333333333333333703, 0.3249759707272745768, 0.3333333333333333703, 0.3249759707272745768, 0.3333333333333333703, 0.3249759707272745768, 0.3333333333333333703, 0.3249759707272745768, 0.3333333333333333703, 0.3249759707272745768, 0.3333333333333333703, 0.3249759707272745768, 0.3333333333333333703, 0.3249759707272745768, 0.3333333333333333703, 0.3249759707272745768, 0.3333333333333333703, 0.3249759707272745768, 0.3333333333333333703, 0.3249759707272745768, 0.3333333333333333703, 0.3249759707272745768, 0.3333333333333333703, 0.3249759707272745768, 0.3333333333333333703, 0.3249759707272745768, 0.3333333333333333703, 0.3249759707272745768, 0.3333333333333333703, 0.3249759707272745768, 0.3333333333333333703, 0.3249759707272745768, 0.3333333333333333703, 0.3249759707272745768, 0.3333333333333333703, 0.3249759707272745768, 0.3333333333333333703, 0.3249759707272745768, 0.3333333333333333703, 0.3249759707272745768, 0.3333333333333333703, 0.3249759707272745768, 0.3333333333333333703, 0.3249759707272745768, 0.3333333333333333703, 0.3249759707272745768, 0.3333333333333333703, 0.3249759707272745768, 0.3333333333333333703, 0.3249759707272745768, 0.3333333333333333703, 0.3249759707272745768, 0.3333333333333333703, 0.3249759707272745768, 0.3333333333333333703, 0.3249759707272745768, 0.3333333333333333703, 0.3249759707272745768, 0.3333333333333333703, 0.3249759707272745768, 0.3333333333333333703, 0.3249759707272745768, 0.3333333333333333703, 0.3249759707272745768, 0.3333333333333333703, 0.3249759707272745768, 0.3333333333333333703, 0.3249759707272745768, 0.3333333333333333703, 0.3249759707272745768, 0.3333333333333333703, 0.3249759707272745768, 0.3333333333333333703, 0.3249759707272745768, 0.3333333333333333703, 0.3249759707272745768, 0.3333333333333333703, 0.3249759707272745768, 0.3333333333333333703, 0.3249759707272745768, 0.3333333333333333703, 0.3249759707272745768, 0.3333333333333333703, 0.3249759707272745768, 0.3333333333333333703, 0.3249759707272745768, 0.3333333333333333703, 0.3249759707272745768, 0.3333333333333333703, 0.3249759707272745768, 0.3333333333333333703, 0.3249759707272745768, 0.3333333333333333703, 0.3249759707272745768, 0.3333333333333333703, 0.3249759707272745768, 0.3333333333333333703, 0.3249759707272745768, 0.3333333333333333703, 0.3249759707272745768, 0.3333333333333333703, 0.3249759707272745768, 0.3333333333333333703, 0.3249759707272745768, 0.3333333333333333703, 0.3249759707272745768, 0.3333333333333333703, 0.3249759707272745768, 0.3333333333333333703, 0.3249759707272745768, 0.3333333333333333703, 0.3249759707272745768, 0.3333333333333333703, 0.3249759707272745768, 0.3333333333333333703, 0.3249759707272745768, 0.3333333333333333703, 0.3249759707272745768, 0.3333333333333333703, 0.3249759707272745768, 0.3333333333333333703, 0.3249759707272745768, 0.3333333333333333703, 0.3249759707272745768, 0.3333333333333333703, 0.3249759707272745768, 0.3333333333333333703, 0.3249759707272745768, 0.3333333333333333703, 0.3249759707272745768, 0.3333333333333333703, 0.3249759707272745768, 0.3333333333333333703, 0.3249759707272745768, 0.3333333333333333703, 0.3249759707272745768, 0.3333333333333333703, 0.3249759707272745768, 0.3333333333333333703, 0.3249759707272745768, 0.3333333333333333703, 0.3249759707272745768, 0.3333333333333333703, 0.3249759707272745768, 0.3333333333333333703, 0.3249759707272745768, 0.3333333333333333703, 0.3249759707272745768, 0.3333333333333333703, 0.3249759707272745768, 0.3333333333333333703, 0.3249759707272745768, 0.3333333333333333703, 0.3249759707272745768, 0.3333333333333333703, 0.3249759707272745768, 0.3333333333333333703, 0.3249759707272745768, 0.3333333333333333703, 0.3249759707272745768, 0.3333333333333333703, 0.3249759707272745768, 0.3333333333333333703, 0.3249759707272745768, 0.3333333333333333703, 0.3249759707272745768, 0.3333333333333333703, 0.3249759707272745768, 0.3333333333333333703, 0.3249759707272745768, 0.3333333333333333703, 0.3249759707272745768, 0.3333333333333333703, 0.3249759707272745768, 0.3333333333333333703, 0.3249759707272745768, 0.3333333333333333703, 0.3249759707272745768, 0.3333333333333333703, 0.3249759707272745768, 0.3333333333333333703, 0.3249759707272745768, 0.3333333333333333703, 0.3249759707272745768, 0.3333333333333333703, 0.3249759707272745768, 0.3333333333333333703, 0.3249759707272745768, 0.3333333333333333703, 0.3249759707272745768, 0.3333333333333333703, 0.3249759707272745768, 0.3333333333333333703, 0.3249759707272745768, 0.3333333333333333703, 0.3249759707272745768, 0.3333333333333333703, 0.3249759707272745768, 0.3333333333333333703, 0.3249759707272745768, 0.3333333333333333703, 0.3249759707272745768, 0.3333333333333333703, 0.3249759707272745768, 0.3333333333333333703, 0.3249759707272745768, 0.3333333333333333703, 0.3249759707272745768, 0.3333333333333333703, 0.3249759707272745768, 0.3333333333333333703, 0.3249759707272745768, 0.3333333333333333703, 0.3249759707272745768, 0.3333333333333333703, 0.3291546520303039736, 0.3291546520303039736),
 ( 0.3333333333333333703, 0.3249759707272745768, 0.3333333333333333703, 0.3249759707272745768, 0.3333333333333333703, 0.3249759707272745768, 0.3333333333333333703, 0.3249759707272745768, 0.3333333333333333703, 0.3249759707272745768, 0.3333333333333333703, 0.3249759707272745768, 0.3333333333333333703, 0.3249759707272745768, 0.3333333333333333703, 0.3249759707272745768, 0.3333333333333333703, 0.3249759707272745768, 0.3333333333333333703, 0.3249759707272745768, 0.3333333333333333703, 0.3249759707272745768, 0.3333333333333333703, 0.3249759707272745768, 0.3333333333333333703, 0.3249759707272745768, 0.3333333333333333703, 0.3249759707272745768, 0.3333333333333333703, 0.3249759707272745768, 0.3333333333333333703, 0.3249759707272745768, 0.3333333333333333703, 0.3249759707272745768, 0.3333333333333333703, 0.3249759707272745768, 0.3333333333333333703, 0.3249759707272745768, 0.3333333333333333703, 0.3249759707272745768, 0.3333333333333333703, 0.3249759707272745768, 0.3333333333333333703, 0.3249759707272745768, 0.3333333333333333703, 0.3249759707272745768, 0.3333333333333333703, 0.3249759707272745768, 0.3333333333333333703, 0.3249759707272745768, 0.3333333333333333703, 0.3249759707272745768, 0.3333333333333333703, 0.3249759707272745768, 0.3333333333333333703, 0.3249759707272745768, 0.3333333333333333703, 0.3249759707272745768, 0.3333333333333333703, 0.3249759707272745768, 0.3333333333333333703, 0.3249759707272745768, 0.3333333333333333703, 0.3249759707272745768, 0.3333333333333333703, 0.3249759707272745768, 0.3333333333333333703, 0.3249759707272745768, 0.3333333333333333703, 0.3249759707272745768, 0.3333333333333333703, 0.3249759707272745768, 0.3333333333333333703, 0.3249759707272745768, 0.3333333333333333703, 0.3249759707272745768, 0.3333333333333333703, 0.3249759707272745768, 0.3333333333333333703, 0.3249759707272745768, 0.3333333333333333703, 0.3249759707272745768, 0.3333333333333333703, 0.3249759707272745768, 0.3333333333333333703, 0.3249759707272745768, 0.3333333333333333703, 0.3249759707272745768, 0.3333333333333333703, 0.3249759707272745768, 0.3333333333333333703, 0.3249759707272745768, 0.3333333333333333703, 0.3249759707272745768, 0.3333333333333333703, 0.3249759707272745768, 0.3333333333333333703, 0.3249759707272745768, 0.3333333333333333703, 0.3249759707272745768, 0.3333333333333333703, 0.3249759707272745768, 0.3333333333333333703, 0.3249759707272745768, 0.3333333333333333703, 0.3249759707272745768, 0.3333333333333333703, 0.3249759707272745768, 0.3333333333333333703, 0.3249759707272745768, 0.3333333333333333703, 0.3249759707272745768, 0.3333333333333333703, 0.3249759707272745768, 0.3333333333333333703, 0.3249759707272745768, 0.3333333333333333703, 0.3249759707272745768, 0.3333333333333333703, 0.3249759707272745768, 0.3333333333333333703, 0.3249759707272745768, 0.3333333333333333703, 0.3249759707272745768, 0.3333333333333333703, 0.3249759707272745768, 0.3333333333333333703, 0.3249759707272745768, 0.3333333333333333703, 0.3249759707272745768, 0.3333333333333333703, 0.3249759707272745768, 0.3333333333333333703, 0.3249759707272745768, 0.3333333333333333703, 0.3249759707272745768, 0.3333333333333333703, 0.3249759707272745768, 0.3333333333333333703, 0.3249759707272745768, 0.3333333333333333703, 0.3249759707272745768, 0.3333333333333333703, 0.3249759707272745768, 0.3333333333333333703, 0.3249759707272745768, 0.3333333333333333703, 0.3249759707272745768, 0.3333333333333333703, 0.3249759707272745768, 0.3333333333333333703, 0.3249759707272745768, 0.3333333333333333703, 0.3249759707272745768, 0.3333333333333333703, 0.3249759707272745768, 0.3333333333333333703, 0.3249759707272745768, 0.3333333333333333703, 0.3249759707272745768, 0.3333333333333333703, 0.3249759707272745768, 0.3333333333333333703, 0.3249759707272745768, 0.3333333333333333703, 0.3249759707272745768, 0.3333333333333333703, 0.3249759707272745768, 0.3333333333333333703, 0.3249759707272745768, 0.3333333333333333703, 0.3249759707272745768, 0.3333333333333333703, 0.3249759707272745768, 0.3333333333333333703, 0.3249759707272745768, 0.3333333333333333703, 0.3249759707272745768, 0.3333333333333333703, 0.3249759707272745768, 0.3333333333333333703, 0.3249759707272745768, 0.3333333333333333703, 0.3249759707272745768, 0.3333333333333333703, 0.3249759707272745768, 0.3333333333333333703, 0.3249759707272745768, 0.3333333333333333703, 0.3249759707272745768, 0.3333333333333333703, 0.3249759707272745768, 0.3333333333333333703, 0.3249759707272745768, 0.3333333333333333703, 0.3249759707272745768, 0.3333333333333333703, 0.3249759707272745768, 0.3333333333333333703, 0.3249759707272745768, 0.3333333333333333703, 0.3249759707272745768, 0.3333333333333333703, 0.3249759707272745768, 0.3333333333333333703, 0.3249759707272745768, 0.3333333333333333703, 0.3249759707272745768, 0.3333333333333333703, 0.3249759707272745768, 0.3333333333333333703, 0.3249759707272745768, 0.3333333333333333703, 0.3249759707272745768, 0.3333333333333333703, 0.3249759707272745768, 0.3333333333333333703, 0.3249759707272745768, 0.3333333333333333703, 0.3249759707272745768, 0.3333333333333333703, 0.3249759707272745768, 0.3333333333333333703, 0.3249759707272745768, 0.3333333333333333703, 0.3249759707272745768, 0.3333333333333333703, 0.3249759707272745768, 0.3333333333333333703, 0.3249759707272745768, 0.3333333333333333703, 0.3291546520303039736, 0.3291546520303039736),
 ( 1.000000000000000000, 0.9749279121818236193, 1.000000000000000000, 0.9749279121818236193, 1.000000000000000000, 0.9749279121818236193, 1.000000000000000000, 0.9749279121818236193, 1.000000000000000000, 0.9749279121818236193, 1.000000000000000000, 0.9749279121818236193, 1.000000000000000000, 0.9749279121818236193, 1.000000000000000000, 0.9749279121818236193, 1.000000000000000000, 0.9749279121818236193, 1.000000000000000000, 0.9749279121818236193, 1.000000000000000000, 0.9749279121818236193, 1.000000000000000000, 0.9749279121818236193, 1.000000000000000000, 0.9749279121818236193, 1.000000000000000000, 0.9749279121818236193, 1.000000000000000000, 0.9749279121818236193, 1.000000000000000000, 0.9749279121818236193, 1.000000000000000000, 0.9749279121818236193, 1.000000000000000000, 0.9749279121818236193, 1.000000000000000000, 0.9749279121818236193, 1.000000000000000000, 0.9749279121818236193, 1.000000000000000000, 0.9749279121818236193, 1.000000000000000000, 0.9749279121818236193, 1.000000000000000000, 0.9749279121818236193, 1.000000000000000000, 0.9749279121818236193, 1.000000000000000000, 0.9749279121818236193, 1.000000000000000000, 0.9749279121818236193, 1.000000000000000000, 0.9749279121818236193, 1.000000000000000000, 0.9749279121818236193, 1.000000000000000000, 0.9749279121818236193, 1.000000000000000000, 0.9749279121818236193, 1.000000000000000000, 0.9749279121818236193, 1.000000000000000000, 0.9749279121818236193, 1.000000000000000000, 0.9749279121818236193, 1.000000000000000000, 0.9749279121818236193, 1.000000000000000000, 0.9749279121818236193, 1.000000000000000000, 0.9749279121818236193, 1.000000000000000000, 0.9749279121818236193, 1.000000000000000000, 0.9749279121818236193, 1.000000000000000000, 0.9749279121818236193, 1.000000000000000000, 0.9749279121818236193, 1.000000000000000000, 0.9749279121818236193, 1.000000000000000000, 0.9749279121818236193, 1.000000000000000000, 0.9749279121818236193, 1.000000000000000000, 0.9749279121818236193, 1.000000000000000000, 0.9749279121818236193, 1.000000000000000000, 0.9749279121818236193, 1.000000000000000000, 0.9749279121818236193, 1.000000000000000000, 0.9749279121818236193, 1.000000000000000000, 0.9749279121818236193, 1.000000000000000000, 0.9749279121818236193, 1.000000000000000000, 0.9749279121818236193, 1.000000000000000000, 0.9749279121818236193, 1.000000000000000000, 0.9749279121818236193, 1.000000000000000000, 0.9749279121818236193, 1.000000000000000000, 0.9749279121818236193, 1.000000000000000000, 0.9749279121818236193, 1.000000000000000000, 0.9749279121818236193, 1.000000000000000000, 0.9749279121818236193, 1.000000000000000000, 0.9749279121818236193, 1.000000000000000000, 0.9749279121818236193, 1.000000000000000000, 0.9749279121818236193, 1.000000000000000000, 0.9749279121818236193, 1.000000000000000000, 0.9749279121818236193, 1.000000000000000000, 0.9749279121818236193, 1.000000000000000000, 0.9749279121818236193, 1.000000000000000000, 0.9749279121818236193, 1.000000000000000000, 0.9749279121818236193, 1.000000000000000000, 0.9749279121818236193, 1.000000000000000000, 0.9749279121818236193, 1.000000000000000000, 0.9749279121818236193, 1.000000000000000000, 0.9749279121818236193, 1.000000000000000000, 0.9749279121818236193, 1.000000000000000000, 0.9749279121818236193, 1.000000000000000000, 0.9749279121818236193, 1.000000000000000000, 0.9749279121818236193, 1.000000000000000000, 0.9749279121818236193, 1.000000000000000000, 0.9749279121818236193, 1.000000000000000000, 0.9749279121818236193, 1.000000000000000000, 0.9749279121818236193, 1.000000000000000000, 0.9749279121818236193, 1.000000000000000000, 0.9749279121818236193, 1.000000000000000000, 0.9749279121818236193, 1.000000000000000000, 0.9749279121818236193, 1.000000000000000000, 0.9749279121818236193, 1.000000000000000000, 0.9749279121818236193, 1.000000000000000000, 0.9749279121818236193, 1.000000000000000000, 0.9749279121818236193, 1.000000000000000000, 0.9749279121818236193, 1.000000000000000000, 0.9749279121818236193, 1.000000000000000000, 0.9749279121818236193, 1.000000000000000000, 0.9749279121818236193, 1.000000000000000000, 0.9749279121818236193, 1.000000000000000000, 0.9749279121818236193, 1.000000000000000000, 0.9749279121818236193, 1.000000000000000000, 0.9749279121818236193, 1.000000000000000000, 0.9749279121818236193, 1.000000000000000000, 0.9749279121818236193, 1.000000000000000000, 0.9749279121818236193, 1.000000000000000000, 0.9749279121818236193, 1.000000000000000000, 0.9749279121818236193, 1.000000000000000000, 0.9749279121818236193, 1.000000000000000000, 0.9749279121818236193, 1.000000000000000000, 0.9749279121818236193, 1.000000000000000000, 0.9749279121818236193, 1.000000000000000000, 0.9749279121818236193, 1.000000000000000000, 0.9749279121818236193, 1.000000000000000000, 0.9749279121818236193, 1.000000000000000000, 0.9749279121818236193, 1.000000000000000000, 0.9749279121818236193, 1.000000000000000000, 0.9749279121818236193, 1.000000000000000000, 0.9749279121818236193, 1.000000000000000000, 0.9749279121818236193, 1.000000000000000000, 0.9749279121818236193, 1.000000000000000000, 0.9749279121818236193, 1.000000000000000000, 0.9749279121818236193, 1.000000000000000000, 0.9874639560909117542, 0.9874639560909117542) ) ) 
 REPRESENTATION_ITEM ( '' )  SURFACE ( )  );
#7386 = SURFACE_STYLE_FILL_AREA ( #4233 ) ;
#7387 = CARTESIAN_POINT ( 'NONE',  ( -166.3117586239410457, 1.006644598837332039, 12.96127626484980233 ) ) ;
#7388 = CARTESIAN_POINT ( 'NONE',  ( 14.28433602490915000, -1.478298951650544479, 34.35310228751642825 ) ) ;
#7389 = CARTESIAN_POINT ( 'NONE',  ( 7.806708723663831506, 7.806708723663930982, 0.7499999999999762412 ) ) ;
#7390 = CARTESIAN_POINT ( 'NONE',  ( -1.595456901104623348, 10.37818827243067155, 8.301137918078554279 ) ) ;
#7391 = ORIENTED_EDGE ( 'NONE', *, *, #3324, .F. ) ;
#7392 = DIRECTION ( 'NONE',  ( 0.000000000000000000, 0.000000000000000000, 1.000000000000000000 ) ) ;
#7393 = CARTESIAN_POINT ( 'NONE',  ( -10.24623928997352351, -10.06191849875416899, 14.50404056962643651 ) ) ;
#7394 = PRESENTATION_STYLE_ASSIGNMENT (( #9009 ) ) ;
#7395 = PRODUCT_DEFINITION_SHAPE ( 'NONE', 'NONE',  #10229 ) ;
#7396 = CARTESIAN_POINT ( 'NONE',  ( -12.08964793087886314, 7.750357176954159932, 21.78975485534072476 ) ) ;
#7397 = CARTESIAN_POINT ( 'NONE',  ( -9.837026868206066865, 5.012215536711416064, 11.84999999999997478 ) ) ;
#7398 = CARTESIAN_POINT ( 'NONE',  ( 8.404922754268618235, 13.61519076058357491, 39.28167371608785174 ) ) ;
#7399 = CARTESIAN_POINT ( 'NONE',  ( -0.3453160816774686892, 15.99627321608801367, 48.73000000000002530 ) ) ;
#7400 = CARTESIAN_POINT ( 'NONE',  ( -8.841785722321695573, 13.82664651025757152, 8.210245144659282346 ) ) ;
#7401 = DIRECTION ( 'NONE',  ( -1.000000000000000000, 1.842239752758738928E-31, -1.780435181894459419E-32 ) ) ;
#7402 = CARTESIAN_POINT ( 'NONE',  ( -163.9214193032601656, -1.865165441064630780, 14.88379409306876866 ) ) ;
#7403 = CARTESIAN_POINT ( 'NONE',  ( -8.486213763410637156, -4.270415729527909043, 7.401137918078573463 ) ) ;
#7404 = CARTESIAN_POINT ( 'NONE',  ( 1.562606840307832368, 9.865911304835510265, 15.44999999999997797 ) ) ;
#7405 = CARTESIAN_POINT ( 'NONE',  ( -166.9318441561673012, 0.9541142454723345878, 14.97019227849299128 ) ) ;
#7406 = CARTESIAN_POINT ( 'NONE',  ( 15.53355953199861794, 5.297344310588528060, 35.93261199819787066 ) ) ;
#7407 = CARTESIAN_POINT ( 'NONE',  ( -7.639999817571787588, 12.15899005565156266, 24.21428571428571530 ) ) ;
#7408 = CARTESIAN_POINT ( 'NONE',  ( 9.899494936611718643, -9.899494936611608509, 39.00000000000000000 ) ) ;
#7409 = ORIENTED_EDGE ( 'NONE', *, *, #6644, .T. ) ;
#7410 = CARTESIAN_POINT ( 'NONE',  ( -5.420364854931999155, -15.49051278174644253, 46.07142857142856940 ) ) ;
#7411 = DIRECTION ( 'NONE',  ( 0.000000000000000000, 0.000000000000000000, 1.000000000000000000 ) ) ;
#7412 = CARTESIAN_POINT ( 'NONE',  ( -15.49051278174638036, -5.420364854932175902, 22.92857142857142705 ) ) ;
#7413 = CARTESIAN_POINT ( 'NONE',  ( 5.110041130070070992, -16.97680807127747826, -1.270000000000007123 ) ) ;
#7414 = CARTESIAN_POINT ( 'NONE',  ( 1.533232399700100945, -9.375578539472067874, 14.79886208192143471 ) ) ;
#7415 = CARTESIAN_POINT ( 'NONE',  ( 9.858066664633883036, 1.612135949262857526, 5.048862081921459577 ) ) ;
#7416 = UNCERTAINTY_MEASURE_WITH_UNIT (LENGTH_MEASURE( 1.000000000000000082E-05 ), #3591, 'distance_accuracy_value', 'NONE');
#7417 = CARTESIAN_POINT ( 'NONE',  ( -1.917699372585823570, -15.88516839912900558, 7.861183426769288829 ) ) ;
#7418 = CARTESIAN_POINT ( 'NONE',  ( -1.837501619626328297, 16.30827793483733856, 24.64285714285714235 ) ) ;
#7419 = DIRECTION ( 'NONE',  ( 1.000000000000000000, 0.000000000000000000, 0.000000000000000000 ) ) ;
#7420 = CARTESIAN_POINT ( 'NONE',  ( 1.707986654103998303, -16.32287076676380266, 7.646897712483577969 ) ) ;
#7421 = PRESENTATION_LAYER_ASSIGNMENT (  '', '', ( #6274 ) ) ;
#7422 = CARTESIAN_POINT ( 'NONE',  ( -12.15899005565164792, 7.639999817571651697, 17.78571428571428115 ) ) ;
#7423 = ADVANCED_FACE ( 'NONE', ( #9229 ), #6006, .T. ) ;
#7424 = CARTESIAN_POINT ( 'NONE',  ( 15.49051278174638036, 5.420364854932175014, 7.928571428571430602 ) ) ;
#7425 = CARTESIAN_POINT ( 'NONE',  ( -1.677562661911643938, -10.91227292449344688, 5.948862081921430622 ) ) ;
#7426 = ORIENTED_EDGE ( 'NONE', *, *, #2922, .T. ) ;
#7427 = CARTESIAN_POINT ( 'NONE',  ( 13.21436662431716869, -4.623906867372263640, 14.57142857142856940 ) ) ;
#7428 = CARTESIAN_POINT ( 'NONE',  ( 15.89939535829187278, 1.791431617653015174, 26.14285714285714590 ) ) ;
#7429 = AXIS2_PLACEMENT_3D ( 'NONE', #8755, #1683, #4826 ) ;
#7430 = VECTOR ( 'NONE', #3112, 1000.000000000000227 ) ;
#7431 = CARTESIAN_POINT ( 'NONE',  ( 7.340858601237956194, 11.92174236212700045, 3.281673716087854409 ) ) ;
#7432 = CARTESIAN_POINT ( 'NONE',  ( -7.806708723663830618, -7.806708723663901672, 11.24999999999999467 ) ) ;
#7433 = CARTESIAN_POINT ( 'NONE',  ( 1.607813917173037899, -14.26974319298267169, 9.642857142857144126 ) ) ;
#7434 = AXIS2_PLACEMENT_3D ( 'NONE', #8506, #8662, #7830 ) ;
#7435 = ADVANCED_FACE ( 'NONE', ( #2145 ), #6054, .T. ) ;
#7436 = CONICAL_SURFACE ( 'NONE', #3988, 1.649999999999984812, 1.029744258676650093 ) ;
#7437 = CARTESIAN_POINT ( 'NONE',  ( -12.22833218042443271, 7.529642458189139909, 31.78167371608784819 ) ) ;
#7438 = CARTESIAN_POINT ( 'NONE',  ( 10.90442828429184274, 1.727091770866679310, 19.04999999999997939 ) ) ;
#7439 = PRODUCT_RELATED_PRODUCT_CATEGORY ( 'part', '', ( #7568 ) ) ;
#7440 = CARTESIAN_POINT ( 'NONE',  ( -166.4829340271541582, 0.7315032035247491793, 12.97978828447449828 ) ) ;
#7441 = CARTESIAN_POINT ( 'NONE',  ( -1.513077731352923339, -9.873755945037078874, 2.948862081921438616 ) ) ;
#7442 = CARTESIAN_POINT ( 'NONE',  ( 12.22833218042443271, -7.529642458189144349, 46.78167371608785885 ) ) ;
#7443 = CARTESIAN_POINT ( 'NONE',  ( 7.842167650704563897, 7.771249796623195039, 14.75113791807856956 ) ) ;
#7444 = CARTESIAN_POINT ( 'NONE',  ( 9.377220287599001836, 4.724406229267489543, -0.09886208192143307316 ) ) ;
#7445 = MECHANICAL_DESIGN_GEOMETRIC_PRESENTATION_REPRESENTATION (  '', ( #3453 ), #357 ) ;
#7446 = STYLED_ITEM ( 'NONE', ( #6407 ), #8455 ) ;
#7447 = CARTESIAN_POINT ( 'NONE',  ( -58.00000000000001421, 8.200000000000001066, 0.000000000000000000 ) ) ;
#7448 = CARTESIAN_POINT ( 'NONE',  ( -13.59724543428031573, -4.619798703722008959, 20.93261199819787066 ) ) ;
#7449 = CARTESIAN_POINT ( 'NONE',  ( -5.012215536711506658, 9.837026868206027785, 12.14999999999996305 ) ) ;
#7450 = CARTESIAN_POINT ( 'NONE',  ( 5.297344310588354865, 15.53355953199867301, 45.06738800180215065 ) ) ;
#7451 = CYLINDRICAL_SURFACE ( 'NONE', #3082, 18.00000000000000355 ) ;
#7452 = PRESENTATION_LAYER_ASSIGNMENT (  '', '', ( #1690 ) ) ;
#7453 = CARTESIAN_POINT ( 'NONE',  ( -8.512513224245306986, -13.54758718765259218, 22.28571428571428470 ) ) ;
#7454 = CARTESIAN_POINT ( 'NONE',  ( 2.000000000000001776, 2.775557561562891351E-14, 1.535499999999967446 ) ) ;
#7455 = CARTESIAN_POINT ( 'NONE',  ( 8.877401133907127928, -4.579542530753020202, 6.351137918078572753 ) ) ;
#7456 = CARTESIAN_POINT ( 'NONE',  ( 9.383039235653818366, -1.486127417882131097, 16.19999999999999218 ) ) ;
#7457 = CARTESIAN_POINT ( 'NONE',  ( 4.200000000000009059, 1.638219973650290020E-33, 2.000000000000000888 ) ) ;
#7458 = CARTESIAN_POINT ( 'NONE',  ( -13.61519076058348254, -8.404922754268771001, 38.71832628391214826 ) ) ;
#7459 = CARTESIAN_POINT ( 'NONE',  ( 12.15899005565164792, -7.639999817571655250, 26.78571428571429536 ) ) ;
#7460 = EDGE_CURVE ( 'NONE', #4209, #1692, #7279, .T. ) ;
#7461 = CARTESIAN_POINT ( 'NONE',  ( 11.85413878919593422, 7.448449071214774619, 43.71428571428572241 ) ) ;
#7462 = ORIENTED_EDGE ( 'NONE', *, *, #2876, .F. ) ;
#7463 = CARTESIAN_POINT ( 'NONE',  ( -11.60466159355861926, -11.60466159355875249, 46.50000000000002132 ) ) ;
#7464 = CARTESIAN_POINT ( 'NONE',  ( -4.995402070941133310, -13.58603705635637304, -1.270000000000007123 ) ) ;
#7465 = CARTESIAN_POINT ( 'NONE',  ( -1.791431617652833763, -15.89939535829188877, 9.857142857142855874 ) ) ;
#7466 = DIRECTION ( 'NONE',  ( -1.000000000000000000, -0.000000000000000000, -0.000000000000000000 ) ) ;
#7467 = CARTESIAN_POINT ( 'NONE',  ( -0.3453160816774686892, 15.99627321608801367, 48.73000000000002530 ) ) ;
#7468 = CARTESIAN_POINT ( 'NONE',  ( 9.858066664633883036, 1.612135949262858858, 14.04886208192143471 ) ) ;
#7469 = CARTESIAN_POINT ( 'NONE',  ( 8.922933199037192509, -4.490180821391404287, 8.348862081921442524 ) ) ;
#7470 = CARTESIAN_POINT ( 'NONE',  ( -16.29368510291090288, 1.967016585148476215, 9.361183426769292382 ) ) ;
#7471 = CARTESIAN_POINT ( 'NONE',  ( -1.791431617652833763, -15.89939535829188877, 27.85714285714285765 ) ) ;
#7472 = CARTESIAN_POINT ( 'NONE',  ( 17.72919999999999874, -4.025229594467098114E-49, 0.000000000000000000 ) ) ;
#7473 = CARTESIAN_POINT ( 'NONE',  ( 1.917699372585825790, 15.88516839912900203, 10.86118342676929238 ) ) ;
#7474 = AXIS2_PLACEMENT_3D ( 'NONE', #1002, #1822, #2597 ) ;
#7475 = CARTESIAN_POINT ( 'NONE',  ( -14.26974319298268767, 1.607813917172874918, 23.35714285714286476 ) ) ;
#7476 = CARTESIAN_POINT ( 'NONE',  ( 15.10213328493390783, -5.284464991282587398, 8.571428571428569398 ) ) ;
#7477 = CARTESIAN_POINT ( 'NONE',  ( -83.00000000000001421, 1.592040838891559095E-15, -13.00000000000000000 ) ) ;
#7478 = ORIENTED_EDGE ( 'NONE', *, *, #9119, .T. ) ;
#7479 = CARTESIAN_POINT ( 'NONE',  ( -7.448449071214644945, -11.85413878919601771, 10.28571428571428648 ) ) ;
#7480 = EDGE_LOOP ( 'NONE', ( #3784, #3296, #92, #2822 ) ) ;
#7481 = CARTESIAN_POINT ( 'NONE',  ( 1.791431617652837316, 15.89939535829188877, 36.85714285714286120 ) ) ;
#7482 = CARTESIAN_POINT ( 'NONE',  ( 1.665163862719847732, 15.91362231745477374, 44.85310228751641404 ) ) ;
#7483 = CARTESIAN_POINT ( 'NONE',  ( 7.424621202458790314, -7.424621202458697944, 19.50000000000001776 ) ) ;
#7484 = PRODUCT ( 'basic internal retaining ring_ai_B27.1 - NA2-131', 'basic internal retaining ring_ai_B27.1 - NA2-131', '', ( #2774 ) ) ;
#7485 = APPLICATION_PROTOCOL_DEFINITION ( 'draft international standard', 'automotive_design', 1998, #5395 ) ;
#7486 = CARTESIAN_POINT ( 'NONE',  ( -4.623906867372410190, 13.21436662431711895, 6.428571428571429713 ) ) ;
#7487 = EDGE_CURVE ( 'NONE', #2833, #2214, #4578, .T. ) ;
#7488 = CARTESIAN_POINT ( 'NONE',  ( 13.51115193377584589, 4.865839792409294873, 21.92453085894500120 ) ) ;
#7489 = AXIS2_PLACEMENT_3D ( 'NONE', #3259, #7190, #6401 ) ;
#7490 = CARTESIAN_POINT ( 'NONE',  ( -55.00000000000002132, 7.703719777548943412E-30, -7.703719777548943412E-31 ) ) ;
#7491 = CARTESIAN_POINT ( 'NONE',  ( -158.0000000000000284, -7.514081744949122117E-15, 0.000000000000000000 ) ) ;
#7492 = CARTESIAN_POINT ( 'NONE',  ( -8.922933199037192509, 4.490180821391428267, 3.848862081921410105 ) ) ;
#7493 = CARTESIAN_POINT ( 'NONE',  ( 9.899494936611718643, -9.899494936611608509, 3.000000000000002665 ) ) ;
#7494 = CARTESIAN_POINT ( 'NONE',  ( -9.355568503977838901, -4.766900247265280832, 2.400000000000013234 ) ) ;
#7495 = CARTESIAN_POINT ( 'NONE',  ( 9.814260835641038128, -5.056896391392198709, 3.351137918078579858 ) ) ;
#7496 = DIRECTION ( 'NONE',  ( -1.000000000000000000, -1.387778780781445676E-16, -0.000000000000000000 ) ) ;
#7497 = CARTESIAN_POINT ( 'NONE',  ( 11.92174236212692229, 7.340858601238088532, 29.71832628391214826 ) ) ;
#7498 =( LENGTH_UNIT ( ) NAMED_UNIT ( * ) SI_UNIT ( .MILLI., .METRE. ) );
#7499 = CARTESIAN_POINT ( 'NONE',  ( -4.865839792409144771, -13.51115193377589740, 26.07546914105500235 ) ) ;
#7500 = CARTESIAN_POINT ( 'NONE',  ( -9.355568503977838901, -4.766900247265280832, 8.399999999999963052 ) ) ;
#7501 = CARTESIAN_POINT ( 'NONE',  ( -15.88516839912898071, -1.917699372586004980, 37.13881657323070584 ) ) ;
#7502 = CARTESIAN_POINT ( 'NONE',  ( -9.131464984045058131, 12.92800615877343517, 48.72999999999997556 ) ) ;
#7503 = CARTESIAN_POINT ( 'NONE',  ( 1.791431617652837316, 15.89939535829188877, 24.85714285714285765 ) ) ;
#7504 = DIRECTION ( 'NONE',  ( 0.000000000000000000, 0.000000000000000000, 1.000000000000000000 ) ) ;
#7505 = CARTESIAN_POINT ( 'NONE',  ( 1.737328882695370558, -14.25515036105620581, 17.63881657323070939 ) ) ;
#7506 = CARTESIAN_POINT ( 'NONE',  ( 9.375578539472099848, -1.533232399699987702, 12.20113791807854398 ) ) ;
#7507 = CARTESIAN_POINT ( 'NONE',  ( -6.717514421272238856, 6.717514421272181124, 18.00000000000001421 ) ) ;
#7508 = DIRECTION ( 'NONE',  ( 0.000000000000000000, -6.338944243255235518E-49, 1.000000000000000000 ) ) ;
#7509 = APPLICATION_CONTEXT ( 'automotive_design' ) ;
#7510 = CARTESIAN_POINT ( 'NONE',  ( 11.69682198916835070, 11.51250119794901394, 35.50404056962644006 ) ) ;
#7511 = CARTESIAN_POINT ( 'NONE',  ( 11.85413878919593422, 7.448449071214774619, 31.71428571428571530 ) ) ;
#7512 = CARTESIAN_POINT ( 'NONE',  ( -14.26974319298268767, 1.607813917172874918, 41.35714285714286120 ) ) ;
#7513 = ORIENTED_EDGE ( 'NONE', *, *, #2011, .F. ) ;
#7514 = CARTESIAN_POINT ( 'NONE',  ( -15.89939535829186923, -1.791431617653016062, 47.14285714285714590 ) ) ;
#7515 = CARTESIAN_POINT ( 'NONE',  ( -8.776584015271360784, 13.37184113485863790, -7.619501960618503881E-17 ) ) ;
#7516 = CARTESIAN_POINT ( 'NONE',  ( -11.31370849898482156, 11.31370849898469544, 36.00000000000000711 ) ) ;
#7517 = DIRECTION ( 'NONE',  ( -1.000000000000000000, 0.000000000000000000, 0.000000000000000000 ) ) ;
#7518 = SURFACE_STYLE_FILL_AREA ( #7625 ) ;
#7519 = LINE ( 'NONE', #3491, #8602 ) ;
#7520 = CARTESIAN_POINT ( 'NONE',  ( -7.027753727702738651, -7.098671581784262941, 15.24886208192144110 ) ) ;
#7521 = CARTESIAN_POINT ( 'NONE',  ( 7.027753727702739539, 7.098671581784282480, 4.748862081921425116 ) ) ;
#7522 = PRODUCT_DEFINITION_CONTEXT ( 'detailed design', #6245, 'design' ) ;
#7523 = CARTESIAN_POINT ( 'NONE',  ( -7.424621202458789426, 7.424621202458723701, 15.00000000000001421 ) ) ;
#7524 = CARTESIAN_POINT ( 'NONE',  ( 13.82664651025767100, -8.841785722321541030, 6.789754855340717654 ) ) ;
#7525 = CARTESIAN_POINT ( 'NONE',  ( 1.791431617652837316, 15.89939535829188877, 30.85714285714286120 ) ) ;
#7526 = CARTESIAN_POINT ( 'NONE',  ( 11.22385875690717683, -11.40355824106234373, 13.00404056962644006 ) ) ;
#7527 = CARTESIAN_POINT ( 'NONE',  ( 13.91197093850538380, 1.567502665446386390, 20.14285714285714235 ) ) ;
#7528 = CARTESIAN_POINT ( 'NONE',  ( 1.837501619626330074, -16.30827793483733501, 3.642857142857144126 ) ) ;
#7529 = CARTESIAN_POINT ( 'NONE',  ( -15.89939535829186923, -1.791431617653016062, 41.14285714285714590 ) ) ;
#7530 = VERTEX_POINT ( 'NONE', #6111 ) ;
#7531 = CARTESIAN_POINT ( 'NONE',  ( -4.623906867372410190, 13.21436662431711895, 18.42857142857143415 ) ) ;
#7532 = ORIENTED_EDGE ( 'NONE', *, *, #5402, .T. ) ;
#7533 = CARTESIAN_POINT ( 'NONE',  ( 15.49051278174637858, 5.420364854932174126, 37.92857142857143060 ) ) ;
#7534 = CARTESIAN_POINT ( 'NONE',  ( -1.441234910513241818, -13.92619789766829008, 5.853102287516418478 ) ) ;
#7535 = CARTESIAN_POINT ( 'NONE',  ( 1.727091770866550968, 10.90442828429186761, 18.44999999999999218 ) ) ;
#7536 = APPLICATION_PROTOCOL_DEFINITION ( 'draft international standard', 'automotive_design', 1998, #6045 ) ;
#7537 = CARTESIAN_POINT ( 'NONE',  ( -12.15899005565164792, 7.639999817571650809, 5.785714285714282923 ) ) ;
#7538 = AXIS2_PLACEMENT_3D ( 'NONE', #2548, #8124, #904 ) ;
#7539 = CARTESIAN_POINT ( 'NONE',  ( -7.750357176954294935, 12.08964793087877787, 26.21024514465928945 ) ) ;
#7540 = VERTEX_POINT ( 'NONE', #3020 ) ;
#7541 = DIRECTION ( 'NONE',  ( -0.000000000000000000, 0.000000000000000000, -1.000000000000000000 ) ) ;
#7542 = PRODUCT_DEFINITION_SHAPE ( 'NONE', 'NONE',  #10238 ) ;
#7543 = CARTESIAN_POINT ( 'NONE',  ( -4.270415729527831772, -8.486213763410678013, 3.098862081921434974 ) ) ;
#7544 = CARTESIAN_POINT ( 'NONE',  ( -1.727091770866549414, -10.90442828429184274, 7.950000000000040146 ) ) ;
#7545 = CARTESIAN_POINT ( 'NONE',  ( 4.809394265263009061, 9.333916720356739916, 5.601137918078562983 ) ) ;
#7546 = DIRECTION ( 'NONE',  ( -4.755747939841216568E-17, 1.000000000000000000, 0.000000000000000000 ) ) ;
#7547 = CARTESIAN_POINT ( 'NONE',  ( 9.809645194534072132, -9.989344678689256796, 31.00404056962644006 ) ) ;
#7548 = ADVANCED_FACE ( 'NONE', ( #7684 ), #1122, .T. ) ;
#7549 = CARTESIAN_POINT ( 'NONE',  ( 7.806708723663831506, 7.806708723663931870, 3.749999999999997335 ) ) ;
#7550 = CARTESIAN_POINT ( 'NONE',  ( 15.44746603149413922, 5.543385399275817527, 45.92453085894500475 ) ) ;
#7551 = EDGE_CURVE ( 'NONE', #2003, #5232, #5130, .T. ) ;
#7552 = DIRECTION ( 'NONE',  ( 0.000000000000000000, -6.338944243255235518E-49, 1.000000000000000000 ) ) ;
#7553 = DIRECTION ( 'NONE',  ( 0.000000000000000000, -1.000000000000000000, 0.000000000000000000 ) ) ;
#7554 = COLOUR_RGB ( '', 0.08235294, 0.09019608, 0.10196078) ;
#7555 = CARTESIAN_POINT ( 'NONE',  ( -13.25633410266679313, 4.503970704919840529, 19.56738800180213644 ) ) ;
#7556 = CARTESIAN_POINT ( 'NONE',  ( 9.375578539472099848, -1.533232399699987702, 15.20113791807854575 ) ) ;
#7557 = CARTESIAN_POINT ( 'NONE',  ( 4.534861676072320158, -8.900167166472098046, 13.65000000000003233 ) ) ;
#7558 = CARTESIAN_POINT ( 'NONE',  ( -166.6190172193898036, 1.421584020712995056, 14.93281639362370328 ) ) ;
#7559 = CARTESIAN_POINT ( 'NONE',  ( -8.621071003556675549, 13.96533075980314642, 40.21832628391215536 ) ) ;
#7560 = CARTESIAN_POINT ( 'NONE',  ( -4.503970704919988854, 13.25633410266674517, -1.567388001802134223 ) ) ;
#7561 = CARTESIAN_POINT ( 'NONE',  ( 1.607813917173038121, -14.26974319298267346, 39.64285714285716722 ) ) ;
#7562 = VERTEX_POINT ( 'NONE', #5295 ) ;
#7563 = AXIS2_PLACEMENT_3D ( 'NONE', #3885, #7812, #7663 ) ;
#7564 = CARTESIAN_POINT ( 'NONE',  ( 11.60466159355862104, 11.60466159355875071, 43.50000000000000711 ) ) ;
#7565 = CARTESIAN_POINT ( 'NONE',  ( -6.919986107680330178, -12.02850919814119557, 0.000000000000000000 ) ) ;
#7566 = CARTESIAN_POINT ( 'NONE',  ( -5.420364854931999155, -15.49051278174644253, 34.07142857142859071 ) ) ;
#7567 = CARTESIAN_POINT ( 'NONE',  ( 5.986002070941135678, -13.58603705635637304, -1.270000000000007123 ) ) ;
#7568 = PRODUCT ( 'cir_block', 'cir_block', '', ( #2058 ) ) ;
#7569 = PRODUCT_DEFINITION ( 'UNKNOWN', '', #2446, #4423 ) ;
#7570 = CARTESIAN_POINT ( 'NONE',  ( -4.766900247265192014, -9.355568503977876205, 2.099999999999990763 ) ) ;
#7571 = CARTESIAN_POINT ( 'NONE',  ( -6.717514421272238856, 6.717514421272176683, 3.000000000000002665 ) ) ;
#7572 = CARTESIAN_POINT ( 'NONE',  ( -4.270415729527831772, -8.486213763410678013, 12.09886208192144252 ) ) ;
#7573 = CARTESIAN_POINT ( 'NONE',  ( -1.727091770866549414, -10.90442828429184630, 16.94999999999998863 ) ) ;
#7574 = CARTESIAN_POINT ( 'NONE',  ( -13.61519076058348254, -8.404922754268771001, 14.71832628391215003 ) ) ;
#7575 = CARTESIAN_POINT ( 'NONE',  ( 15.89939535829187278, 1.791431617653015174, 44.14285714285714590 ) ) ;
#7576 = CARTESIAN_POINT ( 'NONE',  ( 11.22385875690717683, -11.40355824106234373, 7.004040569626434731 ) ) ;
#7577 = CARTESIAN_POINT ( 'NONE',  ( -13.21436662431716869, 4.623906867372262752, 17.57142857142856940 ) ) ;
#7578 = CARTESIAN_POINT ( 'NONE',  ( 11.31370849898482334, -11.31370849898469366, 3.000000000000002665 ) ) ;
#7579 = CARTESIAN_POINT ( 'NONE',  ( -5.284464991282755264, 15.10213328493384743, 48.42857142857143060 ) ) ;
#7580 = ORIENTED_EDGE ( 'NONE', *, *, #7179, .T. ) ;
#7581 = CARTESIAN_POINT ( 'NONE',  ( 9.355568503977840678, 4.766900247265305701, 12.90000000000002345 ) ) ;
#7582 = ORIENTED_EDGE ( 'NONE', *, *, #3485, .T. ) ;
#7583 = CARTESIAN_POINT ( 'NONE',  ( 11.60466159355861926, 11.60466159355874716, 25.50000000000000355 ) ) ;
#7584 = CARTESIAN_POINT ( 'NONE',  ( -15.14410076328353227, 5.164528828830164287, 49.56738800180214355 ) ) ;
#7585 = CARTESIAN_POINT ( 'NONE',  ( -1.642561882922479732, 10.37072757624895303, 15.29999999999997939 ) ) ;
#7586 = APPLICATION_PROTOCOL_DEFINITION ( 'draft international standard', 'automotive_design', 1998, #7716 ) ;
#7587 = CARTESIAN_POINT ( 'NONE',  ( -1.607813917173034124, 14.26974319298267346, 24.64285714285714235 ) ) ;
#7588 = EDGE_CURVE ( 'NONE', #7640, #6295, #9496, .T. ) ;
#7589 = ORIENTED_EDGE ( 'NONE', *, *, #5165, .F. ) ;
#7590 = CARTESIAN_POINT ( 'NONE',  ( -13.51115193377584589, -4.865839792409295761, 36.92453085894499765 ) ) ;
#7591 = VECTOR ( 'NONE', #5714, 999.9999999999998863 ) ;
#7592 = ORIENTED_EDGE ( 'NONE', *, *, #5713, .F. ) ;
#7593 = CARTESIAN_POINT ( 'NONE',  ( 7.424621202458790314, -7.424621202458697944, 19.50000000000001776 ) ) ;
#7594 = CARTESIAN_POINT ( 'NONE',  ( 15.44746603149413922, 5.543385399275817527, 9.924530858944988765 ) ) ;
#7595 = CYLINDRICAL_SURFACE ( 'NONE', #570, 8.000000000000000000 ) ;
#7596 = CARTESIAN_POINT ( 'NONE',  ( 1.513077731352925115, 9.873755945037098414, 4.448862081921434175 ) ) ;
#7597 = CARTESIAN_POINT ( 'NONE',  ( -1.441234910513241818, -13.92619789766829008, 47.85310228751642114 ) ) ;
#7598 = CARTESIAN_POINT ( 'NONE',  ( -7.806708723663830618, -7.806708723663906113, 8.250000000000028422 ) ) ;
#7599 = CARTESIAN_POINT ( 'NONE',  ( 4.967534682030706250, -9.859792900771036983, 15.65113791807858235 ) ) ;
#7600 = DIRECTION ( 'NONE',  ( 0.000000000000000000, -8.191099868251441548E-34, -1.000000000000000000 ) ) ;
#7601 = CARTESIAN_POINT ( 'NONE',  ( 7.529642458189280241, -12.22833218042435099, 31.21832628391215536 ) ) ;
#7602 = AXIS2_PLACEMENT_3D ( 'NONE', #9502, #8511, #2310 ) ;
#7603 = CIRCLE ( 'NONE', #3818, 18.00000000000000355 ) ;
#7604 = CIRCLE ( 'NONE', #3810, 8.200000000000009948 ) ;
#7605 =( NAMED_UNIT ( * ) PLANE_ANGLE_UNIT ( ) SI_UNIT ( $, .RADIAN. ) );
#7606 = ORIENTED_EDGE ( 'NONE', *, *, #5317, .F. ) ;
#7607 = CARTESIAN_POINT ( 'NONE',  ( 10.90442828429183919, 1.727091770866679532, 13.04999999999999538 ) ) ;
#7608 = CARTESIAN_POINT ( 'NONE',  ( 11.51250119794888249, 11.69682198916847682, 33.49595943037355994 ) ) ;
#7609 = CARTESIAN_POINT ( 'NONE',  ( -13.19169480182751464, 7.515308610800390809, 48.73000000000003951 ) ) ;
#7610 = LINE ( 'NONE', #8379, #1865 ) ;
#7611 = CIRCLE ( 'NONE', #689, 1.000000000000000888 ) ;
#7612 = CARTESIAN_POINT ( 'NONE',  ( -7.750357176954294935, 12.08964793087877787, 14.21024514465927702 ) ) ;
#7613 = CARTESIAN_POINT ( 'NONE',  ( 8.486213763410640709, 4.270415729527941018, 11.90113791807857702 ) ) ;
#7614 = CARTESIAN_POINT ( 'NONE',  ( -9.873755945037078874, -1.513077731353020594, 7.551137918078578259 ) ) ;
#7615 = DIRECTION ( 'NONE',  ( 0.000000000000000000, -1.000000000000000000, 8.191099868251446680E-34 ) ) ;
#7616 = CARTESIAN_POINT ( 'NONE',  ( 13.55419868402807992, 4.742819248065648807, 43.92857142857143060 ) ) ;
#7617 = ADVANCED_FACE ( 'NONE', ( #3857 ), #3953, .F. ) ;
#7618 = CARTESIAN_POINT ( 'NONE',  ( 4.503970704919991519, -13.25633410266674517, 1.432611998197868219 ) ) ;
#7619 = ORIENTED_EDGE ( 'NONE', *, *, #837, .F. ) ;
#7620 = CARTESIAN_POINT ( 'NONE',  ( 13.89598863503046111, -8.731428362939032795, 44.78571428571428470 ) ) ;
#7621 = CARTESIAN_POINT ( 'NONE',  ( -7.654268191094239171, 14.02309213130659593, -7.619501960615842708E-17 ) ) ;
#7622 = EDGE_CURVE ( 'NONE', #2214, #2935, #6593, .T. ) ;
#7623 = CARTESIAN_POINT ( 'NONE',  ( -11.31370849898482156, 11.31370849898469544, 24.00000000000000000 ) ) ;
#7624 = LINE ( 'NONE', #8107, #386 ) ;
#7625 = FILL_AREA_STYLE ('',( #4526 ) ) ;
#7626 = CARTESIAN_POINT ( 'NONE',  ( -1.642561882922479732, 10.37072757624895303, 0.2999999999999669598 ) ) ;
#7627 = CIRCLE ( 'NONE', #32, 1.535500000000000087 ) ;
#7628 = CARTESIAN_POINT ( 'NONE',  ( 7.063212654743467489, 7.063212654743553642, 9.749999999999982236 ) ) ;
#7629 = CARTESIAN_POINT ( 'NONE',  ( -1.533232399700100057, 9.375578539472089190, 4.298862081921427603 ) ) ;
#7630 = CARTESIAN_POINT ( 'NONE',  ( 7.806708723663831506, 7.806708723663925653, 15.74999999999996803 ) ) ;
#7631 = AXIS2_PLACEMENT_3D ( 'NONE', #7682, #6880, #6769 ) ;
#7632 = CARTESIAN_POINT ( 'NONE',  ( -15.10213328493390961, 5.284464991282586510, 41.57142857142856940 ) ) ;
#7633 = CARTESIAN_POINT ( 'NONE',  ( -5.543385399275643444, -15.44746603149420494, 26.07546914105500235 ) ) ;
#7634 = EDGE_CURVE ( 'NONE', #3486, #4085, #5453, .T. ) ;
#7635 = CARTESIAN_POINT ( 'NONE',  ( -12.15899005565164792, 7.639999817571651697, 23.78571428571429536 ) ) ;
#7636 = CARTESIAN_POINT ( 'NONE',  ( -16.30827793483735988, 1.837501619626141780, 5.357142857142856762 ) ) ;
#7637 = CARTESIAN_POINT ( 'NONE',  ( -5.420364854931999155, -15.49051278174644253, 46.07142857142856940 ) ) ;
#7638 = ORIENTED_EDGE ( 'NONE', *, *, #7179, .F. ) ;
#7639 = CARTESIAN_POINT ( 'NONE',  ( 10.37072757624895836, -1.642561882922355831, 19.19999999999999574 ) ) ;
#7640 = VERTEX_POINT ( 'NONE', #2353 ) ;
#7641 = DIRECTION ( 'NONE',  ( -4.755747939841215952E-17, 1.000000000000000000, 0.000000000000000000 ) ) ;
#7642 = CARTESIAN_POINT ( 'NONE',  ( 8.404922754268618235, 13.61519076058357491, 51.28167371608785174 ) ) ;
#7643 = CARTESIAN_POINT ( 'NONE',  ( -5.012215536711506658, 9.837026868206022456, 18.15000000000000924 ) ) ;
#7644 = CARTESIAN_POINT ( 'NONE',  ( -5.284464991282755264, 15.10213328493384743, 0.4285714285714309346 ) ) ;
#7645 = CARTESIAN_POINT ( 'NONE',  ( 5.543385399275644332, 15.44746603149420494, 47.07546914105501656 ) ) ;
#7646 = APPLICATION_PROTOCOL_DEFINITION ( 'draft international standard', 'automotive_design', 1998, #8770 ) ;
#7647 = AXIS2_PLACEMENT_3D ( 'NONE', #9120, #5840, #7504 ) ;
#7648 = CARTESIAN_POINT ( 'NONE',  ( 12.15899005565164792, -7.639999817571654361, 20.78571428571428825 ) ) ;
#7649 = ORIENTED_EDGE ( 'NONE', *, *, #6950, .T. ) ;
#7650 = CARTESIAN_POINT ( 'NONE',  ( 12.22833218042443271, -7.529642458189144349, 34.78167371608785885 ) ) ;
#7651 = VERTEX_POINT ( 'NONE', #2966 ) ;
#7652 = FACE_OUTER_BOUND ( 'NONE', #4591, .T. ) ;
#7653 = CARTESIAN_POINT ( 'NONE',  ( -1.967016585148659846, 16.29368510291087091, 20.63881657323070939 ) ) ;
#7654 = CARTESIAN_POINT ( 'NONE',  ( -13.54758718765249625, -8.512513224245459753, 4.714285714285712636 ) ) ;
#7655 =( REPRESENTATION_RELATIONSHIP ('NONE','NONE', #58, #4550 ) REPRESENTATION_RELATIONSHIP_WITH_TRANSFORMATION ( #4595 )SHAPE_REPRESENTATION_RELATIONSHIP( ) );
#7656 = CARTESIAN_POINT ( 'NONE',  ( -6.751237864895158758, 6.683790977649260334, 0.9988620819214170110 ) ) ;
#7657 = EDGE_CURVE ( 'NONE', #9145, #3268, #3142, .T. ) ;
#7658 = CARTESIAN_POINT ( 'NONE',  ( -10.06191849875405531, -10.24623928997363542, 48.49595943037355994 ) ) ;
#7659 = CARTESIAN_POINT ( 'NONE',  ( 7.806708723663831506, 7.806708723663930982, 6.749999999999960032 ) ) ;
#7660 = CARTESIAN_POINT ( 'NONE',  ( -1.595456901104623348, 10.37818827243067155, 17.30113791807856316 ) ) ;
#7661 = DIRECTION ( 'NONE',  ( 0.000000000000000000, 6.338944243255235518E-49, -1.000000000000000000 ) ) ;
#7662 = CARTESIAN_POINT ( 'NONE',  ( 7.529642458189280241, -12.22833218042435099, 25.21832628391215181 ) ) ;
#7663 = DIRECTION ( 'NONE',  ( 0.000000000000000000, 0.000000000000000000, -1.000000000000000000 ) ) ;
#7664 = EDGE_LOOP ( 'NONE', ( #5282, #7391 ) ) ;
#7665 = CARTESIAN_POINT ( 'NONE',  ( 10.37072757624895836, -1.642561882922356498, 16.19999999999999218 ) ) ;
#7666 = CARTESIAN_POINT ( 'NONE',  ( 1.665163862719847732, 15.91362231745477374, 50.85310228751642825 ) ) ;
#7667 = CARTESIAN_POINT ( 'NONE',  ( 4.766900247265192903, 9.355568503977902850, 0.5999999999999894307 ) ) ;
#7668 = CARTESIAN_POINT ( 'NONE',  ( -13.54758718765249625, -8.512513224245459753, 28.71428571428571530 ) ) ;
#7669 = CARTESIAN_POINT ( 'NONE',  ( -108.0000000000000426, 18.00000000000000355, 2.204364238465236217E-15 ) ) ;
#7670 = CIRCLE ( 'NONE', #9154, 13.00000000000000355 ) ;
#7671 = CARTESIAN_POINT ( 'NONE',  ( -12.22833218042443271, 7.529642458189139909, 19.78167371608784819 ) ) ;
#7672 = CARTESIAN_POINT ( 'NONE',  ( 7.842167650704563897, 7.771249796623202144, -0.2488620819214366897 ) ) ;
#7673 = CARTESIAN_POINT ( 'NONE',  ( -8.877401133907129704, 4.579542530753042406, 7.851137918078569200 ) ) ;
#7674 = CYLINDRICAL_SURFACE ( 'NONE', #1826, 15.99999999999999645 ) ;
#7675 = CARTESIAN_POINT ( 'NONE',  ( 11.69682198916835070, 11.51250119794901394, 41.50404056962644006 ) ) ;
#7676 = CARTESIAN_POINT ( 'NONE',  ( 13.91197093850538380, 1.567502665446386390, 44.14285714285714590 ) ) ;
#7677 = CARTESIAN_POINT ( 'NONE',  ( 4.742819248065503146, 13.55419868402813677, 49.07142857142859071 ) ) ;
#7678 = ORIENTED_EDGE ( 'NONE', *, *, #6058, .T. ) ;
#7679 = CARTESIAN_POINT ( 'NONE',  ( 13.96533075980324234, -8.621071003556521006, 10.78167371608784819 ) ) ;
#7680 = CARTESIAN_POINT ( 'NONE',  ( -31.74999999999994316, 0.000000000000000000, 0.000000000000000000 ) ) ;
#7681 = CARTESIAN_POINT ( 'NONE',  ( -5.284464991282755264, 15.10213328493384743, 36.42857142857143060 ) ) ;
#7682 = CARTESIAN_POINT ( 'NONE',  ( -68.00000000000002842, 0.000000000000000000, 0.000000000000000000 ) ) ;
#7683 = SURFACE_STYLE_USAGE ( .BOTH. , #9955 ) ;
#7684 = FACE_OUTER_BOUND ( 'NONE', #5052, .T. ) ;
#7685 = CARTESIAN_POINT ( 'NONE',  ( 4.312909747525650594, 8.464561979789541724, 9.599999999999997868 ) ) ;
#7686 = CARTESIAN_POINT ( 'NONE',  ( -9.858066664633883036, -1.612135949262833323, 15.54886208192143293 ) ) ;
#7687 = CARTESIAN_POINT ( 'NONE',  ( 0.000000000000000000, 0.000000000000000000, 0.000000000000000000 ) ) ;
#7688 = CARTESIAN_POINT ( 'NONE',  ( -13.54758718765249625, -8.512513224245459753, 46.71428571428571530 ) ) ;
#7689 = CARTESIAN_POINT ( 'NONE',  ( -15.06016580658428694, 5.404401153735006957, 21.57546914105500946 ) ) ;
#7690 = CARTESIAN_POINT ( 'NONE',  ( 11.85413878919593422, 7.448449071214774619, 31.71428571428571530 ) ) ;
#7691 = CARTESIAN_POINT ( 'NONE',  ( 5.284464991282756152, -15.10213328493384743, 15.42857142857143060 ) ) ;
#7692 = CARTESIAN_POINT ( 'NONE',  ( -11.60466159355861926, -11.60466159355875249, 46.50000000000002132 ) ) ;
#7693 = ORIENTED_EDGE ( 'NONE', *, *, #2537, .T. ) ;
#7694 = CARTESIAN_POINT ( 'NONE',  ( -7.806708723663830618, -7.806708723663902560, 14.25000000000001243 ) ) ;
#7695 = ORIENTED_EDGE ( 'NONE', *, *, #3301, .T. ) ;
#7696 = CARTESIAN_POINT ( 'NONE',  ( 8.731428362939189114, -13.89598863503035986, 39.21428571428571530 ) ) ;
#7697 = DIRECTION ( 'NONE',  ( 0.000000000000000000, 0.000000000000000000, 1.000000000000000000 ) ) ;
#7698 = CARTESIAN_POINT ( 'NONE',  ( -1.689666864740335228, 10.36326688006723273, 10.29886208192143293 ) ) ;
#7699 = CARTESIAN_POINT ( 'NONE',  ( 5.420364854932001819, 15.49051278174644430, 7.071428571428569398 ) ) ;
#7700 = CARTESIAN_POINT ( 'NONE',  ( 1.707986654103998303, -16.32287076676380266, 43.64689771248358596 ) ) ;
#7701 = DIRECTION ( 'NONE',  ( 0.000000000000000000, 0.000000000000000000, -1.000000000000000000 ) ) ;
#7702 = CARTESIAN_POINT ( 'NONE',  ( -1.607813917173034124, 14.26974319298267346, 18.64285714285715301 ) ) ;
#7703 = CARTESIAN_POINT ( 'NONE',  ( 1.737328882695370558, -14.25515036105620581, 47.63881657323071295 ) ) ;
#7704 = EDGE_LOOP ( 'NONE', ( #1707, #2158 ) ) ;
#7705 = FACE_BOUND ( 'NONE', #261, .T. ) ;
#7706 = CARTESIAN_POINT ( 'NONE',  ( 8.404922754268618235, 13.61519076058357491, 21.28167371608785530 ) ) ;
#7707 = CARTESIAN_POINT ( 'NONE',  ( -11.31370849898482156, 11.31370849898469544, 0.000000000000000000 ) ) ;
#7708 = CARTESIAN_POINT ( 'NONE',  ( 4.579542530753127672, -8.877401133907065756, 8.648862081921430800 ) ) ;
#7709 = CARTESIAN_POINT ( 'NONE',  ( 13.47998361472151529, 8.620103694222146729, 27.71024514465928235 ) ) ;
#7710 = CARTESIAN_POINT ( 'NONE',  ( -7.424621202458789426, 7.424621202458720148, 3.000000000000002665 ) ) ;
#7711 = CARTESIAN_POINT ( 'NONE',  ( 10.36326688006723984, -1.689666864740212215, 12.20113791807854398 ) ) ;
#7712 = LINE ( 'NONE', #5264, #9439 ) ;
#7713 = CARTESIAN_POINT ( 'NONE',  ( -4.503970704919988854, 13.25633410266674517, 28.43261199819786356 ) ) ;
#7714 = VECTOR ( 'NONE', #1864, 1000.000000000000000 ) ;
#7715 = CARTESIAN_POINT ( 'NONE',  ( -7.340858601237953529, -11.92174236212700222, 6.281673716087846415 ) ) ;
#7716 = APPLICATION_CONTEXT ( 'automotive_design' ) ;
#7717 = CARTESIAN_POINT ( 'NONE',  ( 10.90442828429184274, 1.727091770866678422, 4.049999999999988276 ) ) ;
#7718 = CARTESIAN_POINT ( 'NONE',  ( -13.89598863503046111, 8.731428362939027465, 29.78571428571428825 ) ) ;
#7719 = DIRECTION ( 'NONE',  ( -1.000000000000000000, -4.755747939841215952E-17, 0.000000000000000000 ) ) ;
#7720 = CIRCLE ( 'NONE', #4584, 3.500000000000000000 ) ;
#7721 = CARTESIAN_POINT ( 'NONE',  ( 7.340858601237956194, 11.92174236212700045, 21.28167371608785530 ) ) ;
#7722 = CARTESIAN_POINT ( 'NONE',  ( 8.877401133907127928, -4.579542530753017537, 12.35113791807855677 ) ) ;
#7723 = CARTESIAN_POINT ( 'NONE',  ( 6.683790977649321619, -6.751237864895076157, 9.501137918078587319 ) ) ;
#7724 = CARTESIAN_POINT ( 'NONE',  ( -166.7172248328349724, -1.323598984370104814, 12.93397516672917646 ) ) ;
#7725 = CARTESIAN_POINT ( 'NONE',  ( 14.26974319298268767, -1.607813917172876916, 44.35714285714287541 ) ) ;
#7726 = EDGE_CURVE ( 'NONE', #2258, #1499, #8095, .T. ) ;
#7727 = CARTESIAN_POINT ( 'NONE',  ( -9.899494936611716867, 9.899494936611610285, 48.00000000000000000 ) ) ;
#7728 = VERTEX_POINT ( 'NONE', #1482 ) ;
#7729 = CARTESIAN_POINT ( 'NONE',  ( 13.47998361472151529, 8.620103694222146729, 3.710245144659281458 ) ) ;
#7730 = CYLINDRICAL_SURFACE ( 'NONE', #4648, 8.500000000000000000 ) ;
#7731 = CARTESIAN_POINT ( 'NONE',  ( 15.49051278174638036, 5.420364854932175014, 25.92857142857142705 ) ) ;
#7732 = STYLED_ITEM ( 'NONE', ( #765 ), #67 ) ;
#7733 = DIRECTION ( 'NONE',  ( 1.000000000000000000, 4.755747939841215952E-17, -0.000000000000000000 ) ) ;
#7734 = CARTESIAN_POINT ( 'NONE',  ( -6.976602070941134492, -13.58603705635637304, -1.270000000000007123 ) ) ;
#7735 = CARTESIAN_POINT ( 'NONE',  ( -7.424621202458789426, 7.424621202458724589, 0.000000000000000000 ) ) ;
#7736 = CARTESIAN_POINT ( 'NONE',  ( 8.464561979789474222, 4.312909747525755400, 9.900000000000019895 ) ) ;
#7737 = CARTESIAN_POINT ( 'NONE',  ( 1.513077731352925115, 9.873755945037103743, 19.44886208192144039 ) ) ;
#7738 = CARTESIAN_POINT ( 'NONE',  ( 7.424621202458790314, -7.424621202458697944, 19.50000000000001776 ) ) ;
#7739 = CARTESIAN_POINT ( 'NONE',  ( -11.31370849898482156, 11.31370849898469544, 48.00000000000000000 ) ) ;
#7740 = CARTESIAN_POINT ( 'NONE',  ( 1.707986654103998303, -16.32287076676380266, 13.64689771248357708 ) ) ;
#7741 = CARTESIAN_POINT ( 'NONE',  ( 8.512513224245308763, 13.54758718765259040, 13.28571428571429003 ) ) ;
#7742 = LINE ( 'NONE', #4637, #8093 ) ;
#7743 = EDGE_LOOP ( 'NONE', ( #3513, #8357, #2271 ) ) ;
#7744 = CARTESIAN_POINT ( 'NONE',  ( -5.012215536711506658, 9.837026868206027785, 15.14999999999998259 ) ) ;
#7745 = VERTEX_POINT ( 'NONE', #1584 ) ;
#7746 = CARTESIAN_POINT ( 'NONE',  ( -15.49051278174637858, -5.420364854932175014, 40.92857142857143771 ) ) ;
#7747 = CARTESIAN_POINT ( 'NONE',  ( 7.458344646081711105, -7.390897758835786036, 11.49886208192146775 ) ) ;
#7748 = CARTESIAN_POINT ( 'NONE',  ( 15.49051278174638036, 5.420364854932175014, 1.928571428571430380 ) ) ;
#7749 = CARTESIAN_POINT ( 'NONE',  ( 4.623906867372411078, -13.21436662431711717, 27.42857142857143060 ) ) ;
#7750 = EDGE_CURVE ( 'NONE', #4164, #2935, #9391, .T. ) ;
#7751 = CARTESIAN_POINT ( 'NONE',  ( 6.717514421272239744, -6.717514421272154479, 7.500000000000007105 ) ) ;
#7752 = CARTESIAN_POINT ( 'NONE',  ( 12.22833218042443271, -7.529642458189144349, 40.78167371608785885 ) ) ;
#7753 = EDGE_LOOP ( 'NONE', ( #2882, #7908, #4485, #2678 ) ) ;
#7754 = CARTESIAN_POINT ( 'NONE',  ( -31.74999999999994316, 0.000000000000000000, 0.000000000000000000 ) ) ;
#7755 = CARTESIAN_POINT ( 'NONE',  ( 15.44746603149413922, 5.543385399275817527, 21.92453085894500120 ) ) ;
#7756 = CARTESIAN_POINT ( 'NONE',  ( -6.976602070941134492, -13.58603705635637304, -1.270000000000007123 ) ) ;
#7757 = CARTESIAN_POINT ( 'NONE',  ( -13.47998361472151174, -8.620103694222146729, 18.71024514465927879 ) ) ;
#7758 = DIRECTION ( 'NONE',  ( -1.000000000000000000, -1.387778780781445676E-16, 0.000000000000000000 ) ) ;
#7759 = CARTESIAN_POINT ( 'NONE',  ( 10.91227292449344155, 1.677562661911773390, 12.05113791807856671 ) ) ;
#7760 = CARTESIAN_POINT ( 'NONE',  ( 61.99999999999997158, 0.000000000000000000, 8.000000000000000000 ) ) ;
#7761 = CARTESIAN_POINT ( 'NONE',  ( -1.693770420379220099, -13.89774397934251837, 43.86118342676930126 ) ) ;
#7762 = EDGE_CURVE ( 'NONE', #7327, #1139, #4302, .T. ) ;
#7763 = PRESENTATION_STYLE_ASSIGNMENT (( #9320 ) ) ;
#7764 = VECTOR ( 'NONE', #7303, 1000.000000000000000 ) ;
#7765 = CARTESIAN_POINT ( 'NONE',  ( -11.78653521626494793, -7.556039541191465148, 6.710245144659284122 ) ) ;
#7766 = CARTESIAN_POINT ( 'NONE',  ( 1.727091770866551412, 10.90442828429186761, 6.449999999999970868 ) ) ;
#7767 = CARTESIAN_POINT ( 'NONE',  ( 15.89939535829187278, 1.791431617653015174, 26.14285714285714590 ) ) ;
#7768 = DIRECTION ( 'NONE',  ( -1.000000000000000000, -0.000000000000000000, -0.000000000000000000 ) ) ;
#7769 = CARTESIAN_POINT ( 'NONE',  ( 10.06191849875406064, 10.24623928997363187, 27.49595943037356705 ) ) ;
#7770 = CARTESIAN_POINT ( 'NONE',  ( 7.390897758835871301, -7.458344646081617846, 6.501137918078588207 ) ) ;
#7772 = AXIS2_PLACEMENT_3D ( 'NONE', #4202, #9590, #5648 ) ;
#7771 = CARTESIAN_POINT ( 'NONE',  ( 8.486213763410640709, 4.270415729527937465, 5.901137918078571687 ) ) ;
#7773 = AXIS2_PLACEMENT_3D ( 'NONE', #4617, #5339, #3846 ) ;
#7774 = DIRECTION ( 'NONE',  ( 0.000000000000000000, 0.000000000000000000, 1.000000000000000000 ) ) ;
#7775 = CARTESIAN_POINT ( 'NONE',  ( -1.917699372585823570, -15.88516839912900558, 43.86118342676930126 ) ) ;
#7776 = CARTESIAN_POINT ( 'NONE',  ( -13.55419868402807992, -4.742819248065651472, 46.92857142857142350 ) ) ;
#7777 = CARTESIAN_POINT ( 'NONE',  ( -13.21436662431716869, 4.623906867372262752, 47.57142857142857650 ) ) ;
#7778 = VERTEX_POINT ( 'NONE', #5449 ) ;
#7779 = CIRCLE ( 'NONE', #4136, 1.535500000000000087 ) ;
#7780 = CARTESIAN_POINT ( 'NONE',  ( -13.96533075980324234, 8.621071003556515677, 13.78167371608785174 ) ) ;
#7781 = DIRECTION ( 'NONE',  ( 0.000000000000000000, -1.000000000000000000, 0.000000000000000000 ) ) ;
#7782 = AXIS2_PLACEMENT_3D ( 'NONE', #830, #5629, #6344 ) ;
#7783 = CARTESIAN_POINT ( 'NONE',  ( 16.30827793483735633, -1.837501619626142890, 38.35714285714287541 ) ) ;
#7784 = CARTESIAN_POINT ( 'NONE',  ( -88.00000000000002842, 0.000000000000000000, 0.000000000000000000 ) ) ;
#7785 = DIRECTION ( 'NONE',  ( 3.081487911019577365E-32, 0.4999999999999990008, -0.8660254037844391517 ) ) ;
#7786 = CARTESIAN_POINT ( 'NONE',  ( 9.383039235653818366, -1.486127417882129986, 7.199999999999984190 ) ) ;
#7787 = CARTESIAN_POINT ( 'NONE',  ( -6.751237864895158758, 6.683790977649255005, 12.99886208192142512 ) ) ;
#7788 = DIRECTION ( 'NONE',  ( 0.000000000000000000, -6.338944243255235518E-49, 1.000000000000000000 ) ) ;
#7789 = EDGE_CURVE ( 'NONE', #9967, #5977, #7098, .T. ) ;
#7790 = CARTESIAN_POINT ( 'NONE',  ( 8.620103694221997515, 13.47998361472160767, 17.28975485534072121 ) ) ;
#7791 = CARTESIAN_POINT ( 'NONE',  ( 15.49051278174638036, 5.420364854932175014, 43.92857142857143060 ) ) ;
#7792 = STYLED_ITEM ( 'NONE', ( #6168 ), #2413 ) ;
#7793 = CARTESIAN_POINT ( 'NONE',  ( 8.621071003556677326, -13.96533075980314287, 13.21832628391215181 ) ) ;
#7794 = CARTESIAN_POINT ( 'NONE',  ( -15.10213328493390961, 5.284464991282586510, 23.57142857142857650 ) ) ;
#7795 = DIRECTION ( 'NONE',  ( 0.000000000000000000, -1.000000000000000000, 0.000000000000000000 ) ) ;
#7796 = CARTESIAN_POINT ( 'NONE',  ( -10.37072757624895836, 1.642561882922380034, 11.69999999999998863 ) ) ;
#7797 =( LENGTH_UNIT ( ) NAMED_UNIT ( * ) SI_UNIT ( .MILLI., .METRE. ) );
#7798 = CARTESIAN_POINT ( 'NONE',  ( -1.791431617652833763, -15.89939535829188877, 45.85714285714286120 ) ) ;
#7799 = CARTESIAN_POINT ( 'NONE',  ( 5.056896391392317724, -9.814260835640970626, 5.648862081921440570 ) ) ;
#7800 = CARTESIAN_POINT ( 'NONE',  ( 8.620103694221997515, 13.47998361472160767, 47.28975485534072476 ) ) ;
#7801 = CARTESIAN_POINT ( 'NONE',  ( 4.742819248065502258, 13.55419868402813499, 31.07142857142857295 ) ) ;
#7802 = CARTESIAN_POINT ( 'NONE',  ( -14.25515036105622890, 1.737328882695209575, 33.36118342676929416 ) ) ;
#7803 = CARTESIAN_POINT ( 'NONE',  ( 4.312909747525650594, 8.464561979789541724, 6.599999999999994316 ) ) ;
#7804 = CARTESIAN_POINT ( 'NONE',  ( -4.619798703721853528, -13.59724543428036725, 36.06738800180213644 ) ) ;
#7805 = ORIENTED_EDGE ( 'NONE', *, *, #3298, .T. ) ;
#7806 = DIRECTION ( 'NONE',  ( 0.7071067811865519026, -0.7071067811865431318, 0.000000000000000000 ) ) ;
#7807 = CARTESIAN_POINT ( 'NONE',  ( -8.404922754268618235, -13.61519076058357491, 18.28167371608785174 ) ) ;
#7808 = DIRECTION ( 'NONE',  ( 0.000000000000000000, 8.191099868251448390E-34, 1.000000000000000000 ) ) ;
#7809 = CARTESIAN_POINT ( 'NONE',  ( -11.40355824106246807, 11.22385875690704715, 19.99595943037356349 ) ) ;
#7810 = CARTESIAN_POINT ( 'NONE',  ( -1.595456901104623348, 10.37818827243067155, 14.30113791807856316 ) ) ;
#7811 = CARTESIAN_POINT ( 'NONE',  ( 0.000000000000000000, -6.162975822039154730E-30, 20.00000000000001776 ) ) ;
#7812 = DIRECTION ( 'NONE',  ( 1.000000000000000000, 1.387778780781445676E-16, 0.000000000000000000 ) ) ;
#7813 = CARTESIAN_POINT ( 'NONE',  ( 10.06191849875406064, 10.24623928997363187, 9.495959430373563492 ) ) ;
#7814 = CARTESIAN_POINT ( 'NONE',  ( -4.766900247265192014, -9.355568503977867323, 8.099999999999996092 ) ) ;
#7815 = DIRECTION ( 'NONE',  ( 0.000000000000000000, 0.000000000000000000, 1.000000000000000000 ) ) ;
#7816 = CARTESIAN_POINT ( 'NONE',  ( -13.89774397934249706, -1.693770420379375974, 31.13881657323070939 ) ) ;
#7817 = CARTESIAN_POINT ( 'NONE',  ( 4.967534682030706250, -9.859792900771036983, 6.651137918078563693 ) ) ;
#7818 = CARTESIAN_POINT ( 'NONE',  ( -8.877401133907129704, 4.579542530753039742, 1.851137918078540334 ) ) ;
#7819 = CARTESIAN_POINT ( 'NONE',  ( -164.0445443052358314, -1.931192361225922971, 12.85587404590432392 ) ) ;
#7820 = CARTESIAN_POINT ( 'NONE',  ( 8.620103694221997515, 13.47998361472160767, 47.28975485534072476 ) ) ;
#7821 = CARTESIAN_POINT ( 'NONE',  ( -1.693770420379220099, -13.89774397934251837, 7.861183426769288829 ) ) ;
#7822 = CARTESIAN_POINT ( 'NONE',  ( -4.503970704919988854, 13.25633410266674517, 4.432611998197859116 ) ) ;
#7823 = ORIENTED_EDGE ( 'NONE', *, *, #5286, .F. ) ;
#7824 = CARTESIAN_POINT ( 'NONE',  ( 13.47998361472151529, 8.620103694222146729, 15.71024514465927879 ) ) ;
#7825 = DIRECTION ( 'NONE',  ( -0.000000000000000000, -0.000000000000000000, 1.000000000000000000 ) ) ;
#7826 = CARTESIAN_POINT ( 'NONE',  ( 5.420364854932001819, 15.49051278174644430, 37.07142857142857650 ) ) ;
#7827 = DIRECTION ( 'NONE',  ( 0.000000000000000000, -8.191099868251446680E-34, -1.000000000000000000 ) ) ;
#7828 = CARTESIAN_POINT ( 'NONE',  ( 9.865911304835474738, 1.562606840307950051, 16.04999999999995808 ) ) ;
#7829 = CARTESIAN_POINT ( 'NONE',  ( 6.751237864895159646, -6.683790977649233689, 14.49886208192142867 ) ) ;
#7830 = DIRECTION ( 'NONE',  ( 0.000000000000000000, 1.000000000000000000, 0.000000000000000000 ) ) ;
#7831 = DIRECTION ( 'NONE',  ( 0.000000000000000000, 1.387778780781445676E-16, -1.000000000000000000 ) ) ;
#7832 = CARTESIAN_POINT ( 'NONE',  ( 11.69682198916835070, 11.51250119794901394, 23.50404056962643295 ) ) ;
#7833 = CARTESIAN_POINT ( 'NONE',  ( 8.512513224245308763, 13.54758718765259040, 19.28571428571428825 ) ) ;
#7834 = DIRECTION ( 'NONE',  ( 0.000000000000000000, -6.338944243255235518E-49, 1.000000000000000000 ) ) ;
#7835 = CARTESIAN_POINT ( 'NONE',  ( -16.30827793483735988, 1.837501619626141780, 5.357142857142856762 ) ) ;
#7836 =( NAMED_UNIT ( * ) PLANE_ANGLE_UNIT ( ) SI_UNIT ( $, .RADIAN. ) );
#7837 = CARTESIAN_POINT ( 'NONE',  ( 16.30827793483735633, -1.837501619626142890, 44.35714285714286831 ) ) ;
#7838 =( LENGTH_UNIT ( ) NAMED_UNIT ( * ) SI_UNIT ( .MILLI., .METRE. ) );
#7839 = CARTESIAN_POINT ( 'NONE',  ( 9.859792900771104485, -4.967534682030585458, 8.348862081921442524 ) ) ;
#7840 = CARTESIAN_POINT ( 'NONE',  ( 1.791431617652837316, 15.89939535829188877, 6.857142857142860315 ) ) ;
#7841 = CARTESIAN_POINT ( 'NONE',  ( -15.10213328493390961, 5.284464991282586510, 11.57142857142857295 ) ) ;
#7842 = APPLICATION_PROTOCOL_DEFINITION ( 'draft international standard', 'automotive_design', 1998, #451 ) ;
#7843 = CARTESIAN_POINT ( 'NONE',  ( 12.15899005565164792, -7.639999817571654361, 44.78571428571429180 ) ) ;
#7844 = CARTESIAN_POINT ( 'NONE',  ( -13.92619789766827054, -1.441234910513399470, 33.14689771248357886 ) ) ;
#7845 = CARTESIAN_POINT ( 'NONE',  ( 7.063212654743468377, 7.063212654743558083, 12.75000000000000355 ) ) ;
#7846 = CARTESIAN_POINT ( 'NONE',  ( -9.837026868206066865, 5.012215536711416064, 17.85000000000001918 ) ) ;
#7847 = VERTEX_POINT ( 'NONE', #2205 ) ;
#7848 = CARTESIAN_POINT ( 'NONE',  ( 14.26974319298268767, -1.607813917172876916, 8.357142857142855874 ) ) ;
#7849 = ORIENTED_EDGE ( 'NONE', *, *, #1660, .F. ) ;
#7850 = LINE ( 'NONE', #205, #1034 ) ;
#7851 = CARTESIAN_POINT ( 'NONE',  ( 15.88516839912898071, 1.917699372586004092, 22.13881657323070939 ) ) ;
#7852 = CARTESIAN_POINT ( 'NONE',  ( -16.30827793483735988, 1.837501619626141558, 5.357142857142856762 ) ) ;
#7853 = ADVANCED_FACE ( 'NONE', ( #5398 ), #3905, .T. ) ;
#7854 = CARTESIAN_POINT ( 'NONE',  ( -11.51250119794888072, -11.69682198916848037, 30.49595943037356349 ) ) ;
#7855 = DIRECTION ( 'NONE',  ( -1.000000000000000000, -0.000000000000000000, -0.000000000000000000 ) ) ;
#7856 = CARTESIAN_POINT ( 'NONE',  ( 1.642561882922480621, -10.37072757624892638, 4.800000000000026468 ) ) ;
#7857 = CARTESIAN_POINT ( 'NONE',  ( -10.15407889436378852, -10.15407889436390398, 4.500000000000003553 ) ) ;
#7858 =( NAMED_UNIT ( * ) SI_UNIT ( $, .STERADIAN. ) SOLID_ANGLE_UNIT ( ) );
#7859 = ORIENTED_EDGE ( 'NONE', *, *, #4161, .F. ) ;
#7860 = CARTESIAN_POINT ( 'NONE',  ( 11.78653521626494793, 7.556039541191463371, 3.710245144659281458 ) ) ;
#7861 = CARTESIAN_POINT ( 'NONE',  ( 10.37072757624895836, -1.642561882922355831, 1.200000000000034373 ) ) ;
#7862 = PLANE ( 'NONE',  #6160 ) ;
#7863 = CARTESIAN_POINT ( 'NONE',  ( 10.36326688006723984, -1.689666864740212215, 3.201137918078536426 ) ) ;
#7864 = CARTESIAN_POINT ( 'NONE',  ( -7.390897758835869524, 7.458344646081644491, -0.9988620819214586444 ) ) ;
#7865 = CARTESIAN_POINT ( 'NONE',  ( -165.2805265249035074, -2.136232373723711664, 12.82330986584687693 ) ) ;
#7866 = CARTESIAN_POINT ( 'NONE',  ( -1.478298951650703019, 14.28433602490913579, 4.646897712483579745 ) ) ;
#7867 = EDGE_CURVE ( 'NONE', #4989, #8514, #180, .T. ) ;
#7868 = CARTESIAN_POINT ( 'NONE',  ( 11.92174236212692229, 7.340858601238088532, 17.71832628391214826 ) ) ;
#7869 = VERTEX_POINT ( 'NONE', #3122 ) ;
#7870 = CARTESIAN_POINT ( 'NONE',  ( -15.14410076328353227, 5.164528828830164287, 7.567388001802139108 ) ) ;
#7871 = CARTESIAN_POINT ( 'NONE',  ( -108.0000000000000426, 0.000000000000000000, 0.000000000000000000 ) ) ;
#7872 = CARTESIAN_POINT ( 'NONE',  ( -11.31370849898482156, 11.31370849898469544, 42.00000000000000000 ) ) ;
#7873 = CARTESIAN_POINT ( 'NONE',  ( -170.0000000000000284, -8.084771497730068080E-15, 0.000000000000000000 ) ) ;
#7874 = DIRECTION ( 'NONE',  ( -0.000000000000000000, 0.000000000000000000, 1.000000000000000000 ) ) ;
#7875 = CARTESIAN_POINT ( 'NONE',  ( 4.312909747525650594, 8.464561979789532842, 12.59999999999999964 ) ) ;
#7876 = CARTESIAN_POINT ( 'NONE',  ( -4.534861676072319270, 8.900167166472117586, 6.149999999999980815 ) ) ;
#7877 = CARTESIAN_POINT ( 'NONE',  ( -11.60466159355861926, -11.60466159355875249, 34.50000000000000000 ) ) ;
#7878 = DIRECTION ( 'NONE',  ( 1.000000000000000000, 4.755747939841215952E-17, -0.000000000000000000 ) ) ;
#7879 = CARTESIAN_POINT ( 'NONE',  ( -15.91362231745475597, -1.665163862720028254, 33.14689771248357886 ) ) ;
#7880 = CARTESIAN_POINT ( 'NONE',  ( 8.900167166472158442, -4.534861676072210912, 1.350000000000015410 ) ) ;
#7881 = CARTESIAN_POINT ( 'NONE',  ( -15.91362231745475597, -1.665163862720028254, 33.14689771248357886 ) ) ;
#7882 = ADVANCED_FACE ( 'NONE', ( #7049 ), #9342, .F. ) ;
#7883 = CARTESIAN_POINT ( 'NONE',  ( 15.10213328493390783, -5.284464991282587398, 14.57142857142856940 ) ) ;
#7884 = DIRECTION ( 'NONE',  ( 0.000000000000000000, -6.338944243255235518E-49, 1.000000000000000000 ) ) ;
#7885 = CARTESIAN_POINT ( 'NONE',  ( 15.10213328493390783, -5.284464991282587398, 2.571428571428571619 ) ) ;
#7886 =( LENGTH_UNIT ( ) NAMED_UNIT ( * ) SI_UNIT ( .MILLI., .METRE. ) );
#7887 = DIRECTION ( 'NONE',  ( 0.000000000000000000, 0.000000000000000000, 1.000000000000000000 ) ) ;
#7888 = PRODUCT_DEFINITION_FORMATION_WITH_SPECIFIED_SOURCE ( 'ANY', '', #5087, .NOT_KNOWN. ) ;
#7889 = CARTESIAN_POINT ( 'NONE',  ( -9.333916720356675967, -4.809394265263096990, 9.398862081921446787 ) ) ;
#7890 = CARTESIAN_POINT ( 'NONE',  ( -14.25515036105622890, 1.737328882695209575, 45.36118342676930837 ) ) ;
#7891 = CARTESIAN_POINT ( 'NONE',  ( -16.30827793483735988, 1.837501619626141780, 11.35714285714285943 ) ) ;
#7892 = CARTESIAN_POINT ( 'NONE',  ( 1.607813917173037899, -14.26974319298267169, 39.64285714285715301 ) ) ;
#7893 = CARTESIAN_POINT ( 'NONE',  ( 13.17239914596754424, -4.743843029824685864, 30.57546914105500946 ) ) ;
#7894 = CARTESIAN_POINT ( 'NONE',  ( 4.312909747525650594, 8.464561979789541724, 9.599999999999997868 ) ) ;
#7895 = CARTESIAN_POINT ( 'NONE',  ( 7.424621202458790314, -7.424621202458697944, 16.50000000000001421 ) ) ;
#7896 = EDGE_LOOP ( 'NONE', ( #250, #10126 ) ) ;
#7897 = CARTESIAN_POINT ( 'NONE',  ( -7.340858601237953529, -11.92174236212700222, 48.28167371608785174 ) ) ;
#7898 = ORIENTED_EDGE ( 'NONE', *, *, #5911, .F. ) ;
#7899 = FACE_OUTER_BOUND ( 'NONE', #6440, .T. ) ;
#7900 = CARTESIAN_POINT ( 'NONE',  ( -5.404401153735176599, 15.06016580658422477, 32.42453085894499054 ) ) ;
#7901 = CARTESIAN_POINT ( 'NONE',  ( 13.89598863503045933, -8.731428362939032795, 20.78571428571428825 ) ) ;
#7902 = CARTESIAN_POINT ( 'NONE',  ( -15.44746603149413922, -5.543385399275820191, 18.92453085894499409 ) ) ;
#7903 = CARTESIAN_POINT ( 'NONE',  ( 7.806708723663831506, 7.806708723663930982, 0.7499999999999762412 ) ) ;
#7904 = CARTESIAN_POINT ( 'NONE',  ( 4.766900247265192903, 9.355568503977902850, 3.599999999999992095 ) ) ;
#7905 = EDGE_CURVE ( 'NONE', #4852, #285, #6747, .T. ) ;
#7906 = SURFACE_SIDE_STYLE ('',( #6294 ) ) ;
#7907 = EDGE_CURVE ( 'NONE', #3550, #728, #2487, .T. ) ;
#7908 = ORIENTED_EDGE ( 'NONE', *, *, #2228, .T. ) ;
#7909 = CARTESIAN_POINT ( 'NONE',  ( 7.424621202458790314, -7.424621202458697944, 10.50000000000000888 ) ) ;
#7910 = CARTESIAN_POINT ( 'NONE',  ( 11.31370849898482334, -11.31370849898469366, 15.00000000000000000 ) ) ;
#7911 = CARTESIAN_POINT ( 'NONE',  ( -68.00000000000002842, 8.200000000000001066, 0.000000000000000000 ) ) ;
#7912 = CARTESIAN_POINT ( 'NONE',  ( 7.842167650704563897, 7.771249796623202144, 2.751137918078555789 ) ) ;
#7913 = CARTESIAN_POINT ( 'NONE',  ( -6.683790977649319842, 6.751237864895094809, 11.00113791807855002 ) ) ;
#7914 = CARTESIAN_POINT ( 'NONE',  ( -6.919986107680330178, -12.02850919814119557, -1.270000000000007123 ) ) ;
#7915 = CARTESIAN_POINT ( 'NONE',  ( 11.92174236212692229, 7.340858601238088532, 11.71832628391215181 ) ) ;
#7916 = AXIS2_PLACEMENT_3D ( 'NONE', #2350, #3854, #4626 ) ;
#7917 = CARTESIAN_POINT ( 'NONE',  ( -13.59724543428031573, -4.619798703722008959, 8.932611998197868886 ) ) ;
#7918 = ORIENTED_EDGE ( 'NONE', *, *, #4409, .T. ) ;
#7919 = CARTESIAN_POINT ( 'NONE',  ( -5.986002070941133901, -13.58603705635637304, 0.000000000000000000 ) ) ;
#7920 = CARTESIAN_POINT ( 'NONE',  ( -8.841785722321695573, 13.82664651025757152, 2.210245144659280569 ) ) ;
#7921 = FACE_BOUND ( 'NONE', #1397, .T. ) ;
#7922 = FACE_BOUND ( 'NONE', #7896, .T. ) ;
#7923 = TOROIDAL_SURFACE ( 'NONE', #4789, 11.00000000000000355, 2.000000000000000000 ) ;
#7924 = AXIS2_PLACEMENT_3D ( 'NONE', #2027, #481, #10098 ) ;
#7925 = CARTESIAN_POINT ( 'NONE',  ( -8.464561979789474222, -4.312909747525728754, 17.39999999999997016 ) ) ;
#7926 = CARTESIAN_POINT ( 'NONE',  ( 6.717514421272239744, -6.717514421272154479, 7.500000000000007105 ) ) ;
#7927 = EDGE_CURVE ( 'NONE', #6243, #3552, #10210, .T. ) ;
#7928 = DIRECTION ( 'NONE',  ( 0.000000000000000000, 0.000000000000000000, 1.000000000000000000 ) ) ;
#7929 = CARTESIAN_POINT ( 'NONE',  ( -13.82664651025767100, 8.841785722321537477, 27.78975485534072121 ) ) ;
#7930 = CARTESIAN_POINT ( 'NONE',  ( 9.383039235653818366, -1.486127417882129986, 4.199999999999981526 ) ) ;
#7931 = CARTESIAN_POINT ( 'NONE',  ( -5.164528828830334817, 15.14410076328347543, 34.43261199819786356 ) ) ;
#7932 = VECTOR ( 'NONE', #714, 1000.000000000000000 ) ;
#7933 = ORIENTED_EDGE ( 'NONE', *, *, #10033, .F. ) ;
#7934 = EDGE_CURVE ( 'NONE', #8732, #2655, #3632, .T. ) ;
#7935 = CARTESIAN_POINT ( 'NONE',  ( 15.10213328493390783, -5.284464991282587398, 32.57142857142856940 ) ) ;
#7936 = FACE_OUTER_BOUND ( 'NONE', #4050, .T. ) ;
#7937 = CARTESIAN_POINT ( 'NONE',  ( -7.424621202458789426, 7.424621202458724589, -3.058133128536869244E-17 ) ) ;
#7938 = CARTESIAN_POINT ( 'NONE',  ( -43.00000000000002842, 9.473114452887969885E-16, -8.200000000000001066 ) ) ;
#7939 = CARTESIAN_POINT ( 'NONE',  ( -1.677562661911643938, -10.91227292449344688, 17.94886208192144395 ) ) ;
#7940 =( GEOMETRIC_REPRESENTATION_CONTEXT ( 3 ) GLOBAL_UNCERTAINTY_ASSIGNED_CONTEXT ( ( #5756 ) ) GLOBAL_UNIT_ASSIGNED_CONTEXT ( ( #7886, #8670, #10219 ) ) REPRESENTATION_CONTEXT ( 'NONE', 'WORKASPACE' ) );
#7941 = AXIS2_PLACEMENT_3D ( 'NONE', #8342, #5237, #9901 ) ;
#7942 = CARTESIAN_POINT ( 'NONE',  ( -10.89658364409024749, -1.776620879821561694, 15.54886208192143293 ) ) ;
#7943 = CARTESIAN_POINT ( 'NONE',  ( 5.543385399275644332, 15.44746603149420494, -0.9245308589449906522 ) ) ;
#7944 = CARTESIAN_POINT ( 'NONE',  ( 11.31370849898482334, -11.31370849898469366, 15.00000000000000000 ) ) ;
#7945 = ITEM_DEFINED_TRANSFORMATION ( 'NONE', 'NONE', #8720,  #3995 ) ;
#7946 = CARTESIAN_POINT ( 'NONE',  ( -13.21436662431716869, 4.623906867372262752, 35.57142857142857650 ) ) ;
#7947 = CARTESIAN_POINT ( 'NONE',  ( -13.59724543428031573, -4.619798703722008959, 44.93261199819787777 ) ) ;
#7948 = CARTESIAN_POINT ( 'NONE',  ( 10.24623928997352884, 10.06191849875416899, 35.50404056962644006 ) ) ;
#7949 = CARTESIAN_POINT ( 'NONE',  ( 1.486127417882244783, -9.383039235653782839, 10.80000000000003268 ) ) ;
#7950 =( GEOMETRIC_REPRESENTATION_CONTEXT ( 3 ) GLOBAL_UNCERTAINTY_ASSIGNED_CONTEXT ( ( #8240 ) ) GLOBAL_UNIT_ASSIGNED_CONTEXT ( ( #3266, #7605, #4293 ) ) REPRESENTATION_CONTEXT ( 'NONE', 'WORKASPACE' ) );
#7951 = CARTESIAN_POINT ( 'NONE',  ( -5.012215536711506658, 9.837026868206027785, 15.14999999999998259 ) ) ;
#7952 = CARTESIAN_POINT ( 'NONE',  ( -13.51115193377584589, -4.865839792409295761, 48.92453085894499054 ) ) ;
#7953 = EDGE_LOOP ( 'NONE', ( #5415, #7148, #1565, #1345 ) ) ;
#7954 = DIRECTION ( 'NONE',  ( 1.840628461782073167E-32, 6.938893903907220674E-18, 1.000000000000000000 ) ) ;
#7955 = CARTESIAN_POINT ( 'NONE',  ( 13.54758718765249803, 8.512513224245457977, 13.71428571428571352 ) ) ;
#7956 = CARTESIAN_POINT ( 'NONE',  ( -11.51250119794888072, -11.69682198916848037, 42.49595943037355994 ) ) ;
#7957 = DIRECTION ( 'NONE',  ( 0.7063021515967560227, 0.7063021515967630171, 0.04769215134145720486 ) ) ;
#7958 = CARTESIAN_POINT ( 'NONE',  ( -9.355568503977838901, -4.766900247265279944, 5.400000000000016342 ) ) ;
#7959 = CARTESIAN_POINT ( 'NONE',  ( 14.00000000000000533, 1.318767078788482996E-33, 1.610000000000000098 ) ) ;
#7960 = PRESENTATION_STYLE_ASSIGNMENT (( #831 ) ) ;
#7961 = ORIENTED_EDGE ( 'NONE', *, *, #8368, .F. ) ;
#7962 = CARTESIAN_POINT ( 'NONE',  ( 11.78653521626494793, 7.556039541191463371, 15.71024514465927879 ) ) ;
#7963 = CARTESIAN_POINT ( 'NONE',  ( 7.424621202458790314, -7.424621202458697944, 13.50000000000001243 ) ) ;
#7964 = CARTESIAN_POINT ( 'NONE',  ( 5.284464991282756152, -15.10213328493384743, 15.42857142857143060 ) ) ;
#7965 = CARTESIAN_POINT ( 'NONE',  ( -166.0896366705012781, 1.243800164630720406, 12.94059239432925068 ) ) ;
#7966 = CARTESIAN_POINT ( 'NONE',  ( 13.25633410266679313, -4.503970704919842305, 28.56738800180213644 ) ) ;
#7967 = CARTESIAN_POINT ( 'NONE',  ( -9.377220287598998283, -4.724406229267462898, 4.401137918078569022 ) ) ;
#7968 = CARTESIAN_POINT ( 'NONE',  ( -9.375578539472099848, 1.533232399700011461, 13.70113791807854398 ) ) ;
#7969 = DIRECTION ( 'NONE',  ( 0.000000000000000000, -6.338944243255235518E-49, 1.000000000000000000 ) ) ;
#7970 = CARTESIAN_POINT ( 'NONE',  ( 7.556039541191335474, 11.78653521626503320, 5.289754855340725648 ) ) ;
#7971 = CIRCLE ( 'NONE', #3186, 8.500000000000000000 ) ;
#7972 = CARTESIAN_POINT ( 'NONE',  ( -13.17239914596754424, 4.743843029824683200, 15.57546914105500413 ) ) ;
#7973 = EDGE_CURVE ( 'NONE', #1436, #8355, #2381, .T. ) ;
#7974 = ORIENTED_EDGE ( 'NONE', *, *, #6989, .T. ) ;
#7975 = CIRCLE ( 'NONE', #9800, 16.99999999999997868 ) ;
#7976 = DIRECTION ( 'NONE',  ( 0.000000000000000000, 1.000000000000000000, 0.000000000000000000 ) ) ;
#7977 = CARTESIAN_POINT ( 'NONE',  ( 16.30827793483735633, -1.837501619626142890, 44.35714285714287541 ) ) ;
#7978 = CARTESIAN_POINT ( 'NONE',  ( 5.986002070941135678, -13.58603705635637304, -1.270000000000007123 ) ) ;
#7979 = DIRECTION ( 'NONE',  ( -1.000000000000000000, -1.387778780781445676E-16, -0.000000000000000000 ) ) ;
#7980 = CARTESIAN_POINT ( 'NONE',  ( -7.063212654743466601, -7.063212654743531438, 14.25000000000001243 ) ) ;
#7981 = CARTESIAN_POINT ( 'NONE',  ( 9.383039235653818366, -1.486127417882129986, 10.19999999999998685 ) ) ;
#7982 = CARTESIAN_POINT ( 'NONE',  ( -163.2908618794298832, 1.311844299765515753, 12.93416838467167196 ) ) ;
#7983 = CARTESIAN_POINT ( 'NONE',  ( -11.22385875690717327, 11.40355824106234550, 28.00404056962643651 ) ) ;
#7984 = CARTESIAN_POINT ( 'NONE',  ( -1.486127417882243895, 9.383039235653816590, 3.299999999999969624 ) ) ;
#7985 = CARTESIAN_POINT ( 'NONE',  ( 11.22385875690717683, -11.40355824106234373, 31.00404056962644006 ) ) ;
#7986 = VERTEX_POINT ( 'NONE', #6514 ) ;
#7987 = CARTESIAN_POINT ( 'NONE',  ( -11.31370849898482156, 11.31370849898469544, 30.00000000000000355 ) ) ;
#7988 = CARTESIAN_POINT ( 'NONE',  ( 2.000000000000001776, -1.773042676681352292, -1.110223024625156540E-13 ) ) ;
#7989 = CARTESIAN_POINT ( 'NONE',  ( -15.89939535829186923, -1.791431617653016062, 5.142857142857143238 ) ) ;
#7990 = FILL_AREA_STYLE_COLOUR ( '', #1978 ) ;
#7991 = CARTESIAN_POINT ( 'NONE',  ( -7.027753727702738651, -7.098671581784262941, 9.248862081921457090 ) ) ;
#7992 = CARTESIAN_POINT ( 'NONE',  ( -9.859792900771106261, 4.967534682030607662, 15.84886208192146739 ) ) ;
#7993 = CARTESIAN_POINT ( 'NONE',  ( -16.29368510291090288, 1.967016585148476215, 3.361183426769288385 ) ) ;
#7994 = CARTESIAN_POINT ( 'NONE',  ( 8.731428362939190890, -13.89598863503036164, 21.21428571428571885 ) ) ;
#7995 = CARTESIAN_POINT ( 'NONE',  ( -1.607813917173034124, 14.26974319298267346, 42.64285714285714590 ) ) ;
#7996 = CARTESIAN_POINT ( 'NONE',  ( -4.865839792409144771, -13.51115193377589740, 38.07546914105502367 ) ) ;
#7997 = CARTESIAN_POINT ( 'NONE',  ( 1.607813917173038121, -14.26974319298267346, 9.642857142857147679 ) ) ;
#7998 = CARTESIAN_POINT ( 'NONE',  ( -167.1500000000000341, -5.483569848023176209E-15, 13.00000000000000178 ) ) ;
#7999 = CARTESIAN_POINT ( 'NONE',  ( -9.859792900771106261, 4.967534682030611215, 9.848862081921437195 ) ) ;
#8000 = ORIENTED_EDGE ( 'NONE', *, *, #3345, .F. ) ;
#8001 = CARTESIAN_POINT ( 'NONE',  ( -13.21436662431716869, 4.623906867372262752, 5.571428571428574728 ) ) ;
#8002 = CARTESIAN_POINT ( 'NONE',  ( -158.0000000000000284, 12.99999999999999289, 0.000000000000000000 ) ) ;
#8003 = CARTESIAN_POINT ( 'NONE',  ( -16.30827793483735988, 1.837501619626141558, 23.35714285714286120 ) ) ;
#8004 = CARTESIAN_POINT ( 'NONE',  ( -5.404401153735176599, 15.06016580658422477, 44.42453085894499765 ) ) ;
#8005 = CARTESIAN_POINT ( 'NONE',  ( -1.642561882922479732, 10.37072757624895303, 12.29999999999997762 ) ) ;
#8006 = CARTESIAN_POINT ( 'NONE',  ( 10.90442828429183919, 1.727091770866679310, 7.050000000000010481 ) ) ;
#8007 = DIRECTION ( 'NONE',  ( -1.000000000000000000, 0.000000000000000000, 0.000000000000000000 ) ) ;
#8008 = ORIENTED_EDGE ( 'NONE', *, *, #2260, .T. ) ;
#8009 = CARTESIAN_POINT ( 'NONE',  ( -11.78653521626494793, -7.556039541191465148, 12.71024514465927879 ) ) ;
#8010 = CARTESIAN_POINT ( 'NONE',  ( -9.837026868206070418, 5.012215536711416952, 17.85000000000001918 ) ) ;
#8011 = PRODUCT_DEFINITION ( 'UNKNOWN', '', #1132, #7522 ) ;
#8012 = CARTESIAN_POINT ( 'NONE',  ( 4.246973736992224246, -14.10948682827615919, -1.270000000000007123 ) ) ;
#8013 = CARTESIAN_POINT ( 'NONE',  ( 1.441234910513245149, 13.92619789766829008, 32.85310228751642114 ) ) ;
#8014 = CARTESIAN_POINT ( 'NONE',  ( 1.776620879821457333, 10.89658364409028124, 11.45113791807854220 ) ) ;
#8015 = CARTESIAN_POINT ( 'NONE',  ( 1.439022436064387511, -9.390499931835510239, 15.80113791807855961 ) ) ;
#8016 = DIRECTION ( 'NONE',  ( -1.000000000000000000, -1.387778780781445676E-16, -0.000000000000000000 ) ) ;
#8017 = CARTESIAN_POINT ( 'NONE',  ( 1.693770420379222319, 13.89774397934251837, 22.86118342676929061 ) ) ;
#8018 = SURFACE_SIDE_STYLE ('',( #5642 ) ) ;
#8019 = CARTESIAN_POINT ( 'NONE',  ( 10.24623928997352884, 10.06191849875416899, 17.50404056962643651 ) ) ;
#8020 = EDGE_LOOP ( 'NONE', ( #5360, #2973, #9155, #980 ) ) ;
#8021 = CARTESIAN_POINT ( 'NONE',  ( 2.000000000000001776, -0.8865213383406761460, 1.535499999999911935 ) ) ;
#8022 = CARTESIAN_POINT ( 'NONE',  ( 13.96533075980324234, -8.621071003556521006, 10.78167371608784819 ) ) ;
#8023 = CARTESIAN_POINT ( 'NONE',  ( 57.99999999999997158, 0.000000000000000000, 0.000000000000000000 ) ) ;
#8024 = CARTESIAN_POINT ( 'NONE',  ( -70.00000000000001421, 0.000000000000000000, 0.000000000000000000 ) ) ;
#8025 = CARTESIAN_POINT ( 'NONE',  ( -8.900167166472156666, 4.534861676072231340, 14.84999999999999787 ) ) ;
#8026 = CARTESIAN_POINT ( 'NONE',  ( 4.534861676072320158, -8.900167166472098046, 10.65000000000000924 ) ) ;
#8027 = ADVANCED_FACE ( 'NONE', ( #280 ), #1829, .F. ) ;
#8028 = DIRECTION ( 'NONE',  ( 1.000000000000000000, 0.000000000000000000, 0.000000000000000000 ) ) ;
#8029 = CARTESIAN_POINT ( 'NONE',  ( -16.29368510291090288, 1.967016585148476215, 27.36118342676929416 ) ) ;
#8030 = CARTESIAN_POINT ( 'NONE',  ( -4.534861676072319270, 8.900167166472122915, 0.1499999999999952482 ) ) ;
#8031 = CARTESIAN_POINT ( 'NONE',  ( -1.917699372585823570, -15.88516839912900558, 31.86118342676929416 ) ) ;
#8032 = EDGE_CURVE ( 'NONE', #8995, #879, #9592, .T. ) ;
#8033 = CIRCLE ( 'NONE', #1767, 1.816100000000000270 ) ;
#8034 = ADVANCED_FACE ( 'NONE', ( #3275 ), #6416, .T. ) ;
#8035 = ORIENTED_EDGE ( 'NONE', *, *, #5805, .T. ) ;
#8036 = CARTESIAN_POINT ( 'NONE',  ( 5.420364854932001819, 15.49051278174644430, 37.07142857142857650 ) ) ;
#8037 = CARTESIAN_POINT ( 'NONE',  ( -5.543139917359588331, 12.94619968565320711, 3.300085072504093742E-16 ) ) ;
#8038 = CARTESIAN_POINT ( 'NONE',  ( 15.49051278174638036, 5.420364854932175014, 1.928571428571430380 ) ) ;
#8039 = CARTESIAN_POINT ( 'NONE',  ( 9.858066664633883036, 1.612135949262857082, 8.048862081921450695 ) ) ;
#8040 = CARTESIAN_POINT ( 'NONE',  ( -10.37818827243067688, 1.595456901104524761, 18.69886208192145816 ) ) ;
#8041 = CIRCLE ( 'NONE', #7215, 8.200000000000001066 ) ;
#8042 = CARTESIAN_POINT ( 'NONE',  ( 16.29368510291089223, -1.967016585148476882, 0.3611834267692887734 ) ) ;
#8043 = CARTESIAN_POINT ( 'NONE',  ( -8.731428362939189114, 13.89598863503036341, 12.21428571428571885 ) ) ;
#8044 = CARTESIAN_POINT ( 'NONE',  ( 10.15407889436379030, 10.15407889436390221, 43.50000000000000711 ) ) ;
#8045 = CARTESIAN_POINT ( 'NONE',  ( -11.22385875690717327, 11.40355824106234550, -1.995959430373561272 ) ) ;
#8046 = CARTESIAN_POINT ( 'NONE',  ( -13.55419868402807992, -4.742819248065651472, 10.92857142857142883 ) ) ;
#8047 = CARTESIAN_POINT ( 'NONE',  ( 13.61000000000001720, 1.638219973650290362E-33, 2.000000000000001332 ) ) ;
#8048 = CARTESIAN_POINT ( 'NONE',  ( -7.771249796623103556, -7.842167650704634063, 6.248862081921465084 ) ) ;
#8049 = EDGE_LOOP ( 'NONE', ( #4661, #4539 ) ) ;
#8050 = CARTESIAN_POINT ( 'NONE',  ( -4.623906867372410190, 13.21436662431711895, 6.428571428571429713 ) ) ;
#8051 =( GEOMETRIC_REPRESENTATION_CONTEXT ( 3 ) GLOBAL_UNCERTAINTY_ASSIGNED_CONTEXT ( ( #4216 ) ) GLOBAL_UNIT_ASSIGNED_CONTEXT ( ( #3524, #6650, #2736 ) ) REPRESENTATION_CONTEXT ( 'NONE', 'WORKASPACE' ) );
#8052 = CARTESIAN_POINT ( 'NONE',  ( -5.284464991282755264, 15.10213328493384743, 24.42857142857143060 ) ) ;
#8053 = CARTESIAN_POINT ( 'NONE',  ( 8.841785722321695573, -13.82664651025757152, 41.21024514465928235 ) ) ;
#8054 = CARTESIAN_POINT ( 'NONE',  ( -7.806708723663830618, -7.806708723663901672, 5.250000000000008882 ) ) ;
#8055 = CARTESIAN_POINT ( 'NONE',  ( 9.837026868206066865, -5.012215536711392083, 13.34999999999998188 ) ) ;
#8056 = EDGE_CURVE ( 'NONE', #5215, #6370, #7103, .T. ) ;
#8057 = CARTESIAN_POINT ( 'NONE',  ( -83.00000000000001421, 0.000000000000000000, 0.000000000000000000 ) ) ;
#8058 = AXIS2_PLACEMENT_3D ( 'NONE', #2476, #8797, #7701 ) ;
#8059 = EDGE_LOOP ( 'NONE', ( #6387, #9965 ) ) ;
#8060 = CARTESIAN_POINT ( 'NONE',  ( -7.750357176954294935, 12.08964793087877787, 14.21024514465927702 ) ) ;
#8061 = CARTESIAN_POINT ( 'NONE',  ( 9.837026868206070418, -5.012215536711391195, 10.35000000000002274 ) ) ;
#8062 = CARTESIAN_POINT ( 'NONE',  ( -15.10213328493390961, 5.284464991282586510, 11.57142857142857295 ) ) ;
#8063 = DIRECTION ( 'NONE',  ( 0.000000000000000000, 6.938893903907221444E-18, 1.000000000000000000 ) ) ;
#8064 = CARTESIAN_POINT ( 'NONE',  ( 12.22833218042443271, -7.529642458189144349, 40.78167371608785885 ) ) ;
#8065 = CARTESIAN_POINT ( 'NONE',  ( -7.842167650704559456, -7.771249796623176387, 16.25113791807856245 ) ) ;
#8066 = CARTESIAN_POINT ( 'NONE',  ( 8.877401133907127928, -4.579542530753017537, 12.35113791807855677 ) ) ;
#8067 = EDGE_CURVE ( 'NONE', #5081, #2751, #679, .T. ) ;
#8068 = DIRECTION ( 'NONE',  ( 0.000000000000000000, 0.000000000000000000, 1.000000000000000000 ) ) ;
#8069 = CARTESIAN_POINT ( 'NONE',  ( 13.92619789766827587, 1.441234910513398582, 18.14689771248357530 ) ) ;
#8070 = ADVANCED_FACE ( 'NONE', ( #3425 ), #172, .F. ) ;
#8071 = CARTESIAN_POINT ( 'NONE',  ( 4.503970704919991519, -13.25633410266674517, 13.43261199819786711 ) ) ;
#8072 = VERTEX_POINT ( 'NONE', #958 ) ;
#8073 = CARTESIAN_POINT ( 'NONE',  ( 2.000000000000001776, 1.773042676681366281, 0.000000000000000000 ) ) ;
#8074 = CARTESIAN_POINT ( 'NONE',  ( -15.44746603149413922, -5.543385399275820191, 6.924530858944994982 ) ) ;
#8075 = CARTESIAN_POINT ( 'NONE',  ( -163.9949573840844437, -1.313015978385311033, 12.93366173934393260 ) ) ;
#8076 = CARTESIAN_POINT ( 'NONE',  ( 7.424621202458790314, -7.424621202458697944, 19.50000000000001776 ) ) ;
#8077 = CARTESIAN_POINT ( 'NONE',  ( 1.439022436064387511, -9.390499931835510239, 6.801137918078597799 ) ) ;
#8078 = CARTESIAN_POINT ( 'NONE',  ( -1.562606840307830591, -9.865911304835476514, 7.950000000000040146 ) ) ;
#8079 = CARTESIAN_POINT ( 'NONE',  ( -163.0677828165198662, 0.9533406220131400710, 12.96565173575652175 ) ) ;
#8080 = CARTESIAN_POINT ( 'NONE',  ( 7.448449071214646722, 11.85413878919601594, 31.28571428571428470 ) ) ;
#8081 = CARTESIAN_POINT ( 'NONE',  ( 1.917699372585825790, 15.88516839912900203, 28.86118342676929416 ) ) ;
#8082 = ORIENTED_EDGE ( 'NONE', *, *, #100, .T. ) ;
#8083 = CIRCLE ( 'NONE', #1323, 0.4999999999999994449 ) ;
#8084 = CARTESIAN_POINT ( 'NONE',  ( -15.49051278174638036, -5.420364854932175902, 34.92857142857145192 ) ) ;
#8085 = FACE_OUTER_BOUND ( 'NONE', #4275, .T. ) ;
#8086 = CARTESIAN_POINT ( 'NONE',  ( -15.89939535829186923, -1.791431617653016062, 17.14285714285713880 ) ) ;
#8087 = SURFACE_SIDE_STYLE ('',( #1788 ) ) ;
#8088 = ADVANCED_FACE ( 'NONE', ( #6563 ), #2402, .F. ) ;
#8089 = SURFACE_STYLE_USAGE ( .BOTH. , #9608 ) ;
#8090 = CARTESIAN_POINT ( 'NONE',  ( 8.900167166472154889, -4.534861676072210912, 1.350000000000015188 ) ) ;
#8091 = CARTESIAN_POINT ( 'NONE',  ( 7.458344646081711105, -7.390897758835786036, 20.49886208192143400 ) ) ;
#8092 = CARTESIAN_POINT ( 'NONE',  ( 13.61519076058348254, 8.404922754268771001, -0.2816737160878517443 ) ) ;
#8093 = VECTOR ( 'NONE', #661, 1000.000000000000000 ) ;
#8094 = CARTESIAN_POINT ( 'NONE',  ( -16.30827793483735988, 1.837501619626141780, 35.35714285714285410 ) ) ;
#8095 = CIRCLE ( 'NONE', #8, 15.44569104238500046 ) ;
#8096 = AXIS2_PLACEMENT_3D ( 'NONE', #9329, #4720, #10197 ) ;
#8097 = CARTESIAN_POINT ( 'NONE',  ( -7.448449071214644945, -11.85413878919601771, 46.28571428571429180 ) ) ;
#8098 = CARTESIAN_POINT ( 'NONE',  ( 4.503970704919991519, -13.25633410266674517, 37.43261199819787066 ) ) ;
#8099 = CARTESIAN_POINT ( 'NONE',  ( 16.30827793483735633, -1.837501619626142890, 38.35714285714287541 ) ) ;
#8100 = CARTESIAN_POINT ( 'NONE',  ( -13.55419868402807992, -4.742819248065651472, 4.928571428571430602 ) ) ;
#8101 = CARTESIAN_POINT ( 'NONE',  ( -7.063212654743467489, -7.063212654743533214, 17.25000000000003197 ) ) ;
#8102 = CARTESIAN_POINT ( 'NONE',  ( 7.458344646081711105, -7.390897758835778930, 5.498862081921462419 ) ) ;
#8103 = ORIENTED_EDGE ( 'NONE', *, *, #8692, .T. ) ;
#8104 = CARTESIAN_POINT ( 'NONE',  ( 13.55419868402807992, 4.742819248065648807, 13.92857142857143238 ) ) ;
#8105 = ORIENTED_EDGE ( 'NONE', *, *, #457, .T. ) ;
#8106 = MECHANICAL_DESIGN_GEOMETRIC_PRESENTATION_REPRESENTATION (  '', ( #2332 ), #5783 ) ;
#8107 = CARTESIAN_POINT ( 'NONE',  ( 6.182472321793581601E-16, -13.00000000000000178, 1.592040838891559293E-15 ) ) ;
#8108 = AXIS2_PLACEMENT_3D ( 'NONE', #7811, #736, #3884 ) ;
#8109 = CARTESIAN_POINT ( 'NONE',  ( -8.512513224245306986, -13.54758718765259218, 22.28571428571428470 ) ) ;
#8110 = CARTESIAN_POINT ( 'NONE',  ( 1.967016585148662289, -16.29368510291087091, 41.63881657323070584 ) ) ;
#8111 = CARTESIAN_POINT ( 'NONE',  ( -4.766900247265192014, -9.355568503977876205, 5.099999999999993427 ) ) ;
#8112 = CARTESIAN_POINT ( 'NONE',  ( 1.727091770866550968, 10.90442828429186761, 18.44999999999999218 ) ) ;
#8113 = CARTESIAN_POINT ( 'NONE',  ( -7.639999817571786700, 12.15899005565156266, 18.21428571428572241 ) ) ;
#8114 = PRESENTATION_LAYER_ASSIGNMENT (  '', '', ( #5948 ) ) ;
#8115 = CARTESIAN_POINT ( 'NONE',  ( 13.89774397934249706, 1.693770420379375308, 16.13881657323070584 ) ) ;
#8116 = CARTESIAN_POINT ( 'NONE',  ( -1.642561882922479732, 10.37072757624896191, 9.299999999999975842 ) ) ;
#8117 = CARTESIAN_POINT ( 'NONE',  ( 0.000000000000000000, 0.000000000000000000, 113.2548339959390518 ) ) ;
#8118 = CLOSED_SHELL ( 'NONE', ( #616, #6081, #8070, #1598, #1296, #3769, #9335, #3002, #7337, #3441, #9909, #1091, #4098, #296, #7423, #10055, #1686, #6060, #9142, #3236, #9723, #5132, #8181, #8583, #9505, #5021, #10223 ) ) ;
#8119 = CARTESIAN_POINT ( 'NONE',  ( -7.750357176954294935, 12.08964793087877787, 38.21024514465928235 ) ) ;
#8120 = CARTESIAN_POINT ( 'NONE',  ( 10.91227292449344155, 1.677562661911773167, 18.05113791807859513 ) ) ;
#8121 = CARTESIAN_POINT ( 'NONE',  ( -10.36326688006724162, 1.689666864740236640, 1.701137918078535094 ) ) ;
#8122 = DIRECTION ( 'NONE',  ( 1.000000000000000000, 4.755747939841215952E-17, -0.000000000000000000 ) ) ;
#8123 = CARTESIAN_POINT ( 'NONE',  ( 4.503970704919991519, -13.25633410266674517, 13.43261199819786711 ) ) ;
#8124 = DIRECTION ( 'NONE',  ( -0.7056782240951970930, 0.7056782240951883223, -0.06353336191096801977 ) ) ;
#8125 = CARTESIAN_POINT ( 'NONE',  ( -8.841785722321695573, 13.82664651025757152, 14.21024514465927702 ) ) ;
#8126 = DIRECTION ( 'NONE',  ( 0.000000000000000000, 1.000000000000000000, 0.000000000000000000 ) ) ;
#8127 = CARTESIAN_POINT ( 'NONE',  ( -165.6923089559685138, -2.040351103243558395, 14.86068369067391792 ) ) ;
#8128 = CARTESIAN_POINT ( 'NONE',  ( -4.355403765523468529, -8.442910196168346815, 10.10113791807856742 ) ) ;
#8129 = CARTESIAN_POINT ( 'NONE',  ( -8.900167166472156666, 4.534861676072234893, 11.84999999999997478 ) ) ;
#8130 = CARTESIAN_POINT ( 'NONE',  ( -58.00000000000001421, 0.000000000000000000, 0.000000000000000000 ) ) ;
#8131 = CARTESIAN_POINT ( 'NONE',  ( -14.26974319298268767, 1.607813917172874918, 35.35714285714285410 ) ) ;
#8132 = CARTESIAN_POINT ( 'NONE',  ( -1.607813917173034124, 14.26974319298267524, 36.64285714285714590 ) ) ;
#8133 = ORIENTED_EDGE ( 'NONE', *, *, #2093, .T. ) ;
#8134 = CARTESIAN_POINT ( 'NONE',  ( -16.30827793483735988, 1.837501619626141780, 35.35714285714285410 ) ) ;
#8135 = DIRECTION ( 'NONE',  ( -1.000000000000000000, -0.000000000000000000, -0.000000000000000000 ) ) ;
#8136 = CARTESIAN_POINT ( 'NONE',  ( 8.731428362939190890, -13.89598863503036164, 15.21428571428571530 ) ) ;
#8137 = DIRECTION ( 'NONE',  ( 0.000000000000000000, -6.338944243255235518E-49, 1.000000000000000000 ) ) ;
#8138 = CARTESIAN_POINT ( 'NONE',  ( 4.270415729527831772, 8.486213763410697553, 16.59886208192144252 ) ) ;
#8139 = CARTESIAN_POINT ( 'NONE',  ( 8.731428362939190890, -13.89598863503036164, 39.21428571428571530 ) ) ;
#8140 = CARTESIAN_POINT ( 'NONE',  ( -9.859792900771106261, 4.967534682030611215, 18.84886208192146029 ) ) ;
#8141 = UNCERTAINTY_MEASURE_WITH_UNIT (LENGTH_MEASURE( 1.000000000000000082E-05 ), #1268, 'distance_accuracy_value', 'NONE');
#8142 = CARTESIAN_POINT ( 'NONE',  ( -15.06016580658428694, 5.404401153735006957, 15.57546914105500413 ) ) ;
#8143 = CARTESIAN_POINT ( 'NONE',  ( -8.731428362939189114, 13.89598863503036341, 24.21428571428571530 ) ) ;
#8144 = CARTESIAN_POINT ( 'NONE',  ( -13.91197093850538380, -1.567502665446387278, 47.14285714285714590 ) ) ;
#8145 = CARTESIAN_POINT ( 'NONE',  ( -16.29368510291090288, 1.967016585148476215, 3.361183426769288385 ) ) ;
#8146 = CARTESIAN_POINT ( 'NONE',  ( 12.15899005565164792, -7.639999817571655250, 8.785714285714293581 ) ) ;
#8147 = CARTESIAN_POINT ( 'NONE',  ( 7.063212654743468377, 7.063212654743554531, 15.74999999999996803 ) ) ;
#8148 = CARTESIAN_POINT ( 'NONE',  ( 10.89658364409024749, 1.776620879821585897, 5.048862081921459577 ) ) ;
#8149 = VERTEX_POINT ( 'NONE', #7156 ) ;
#8150 = CARTESIAN_POINT ( 'NONE',  ( -11.85413878919593422, -7.448449071214776396, 10.71428571428571708 ) ) ;
#8151 = EDGE_LOOP ( 'NONE', ( #8512, #8169, #2382, #364, #9196 ) ) ;
#8152 = CIRCLE ( 'NONE', #10137, 17.72919999999999874 ) ;
#8153 = CARTESIAN_POINT ( 'NONE',  ( -1.837501619626327853, 16.30827793483733856, 30.64285714285714946 ) ) ;
#8154 = CARTESIAN_POINT ( 'NONE',  ( 11.40355824106246985, -11.22385875690704538, 34.99595943037355994 ) ) ;
#8155 = CARTESIAN_POINT ( 'NONE',  ( 10.90442828429183919, 1.727091770866679310, 7.050000000000010481 ) ) ;
#8156 = EDGE_CURVE ( 'NONE', #9145, #9666, #6098, .T. ) ;
#8157 = CARTESIAN_POINT ( 'NONE',  ( -9.899494936611716867, 9.899494936611610285, 11.99999999999999645 ) ) ;
#8158 = CARTESIAN_POINT ( 'NONE',  ( 7.340858601237956194, 11.92174236212700045, 27.28167371608785174 ) ) ;
#8159 = FILL_AREA_STYLE_COLOUR ( '', #3089 ) ;
#8160 = FACE_BOUND ( 'NONE', #5531, .T. ) ;
#8161 = CARTESIAN_POINT ( 'NONE',  ( 10.06191849875406064, 10.24623928997363187, 33.49595943037355994 ) ) ;
#8162 = CARTESIAN_POINT ( 'NONE',  ( 10.36326688006723984, -1.689666864740212215, 15.20113791807854575 ) ) ;
#8163 = CARTESIAN_POINT ( 'NONE',  ( 9.814260835641038128, -5.056896391392198709, 0.3511379180785880183 ) ) ;
#8164 = CARTESIAN_POINT ( 'NONE',  ( 56.99999999999997158, 0.000000000000000000, 0.000000000000000000 ) ) ;
#8165 =( REPRESENTATION_RELATIONSHIP ('NONE','NONE', #58, #8171 ) REPRESENTATION_RELATIONSHIP_WITH_TRANSFORMATION ( #4695 )SHAPE_REPRESENTATION_RELATIONSHIP( ) );
#8166 = CARTESIAN_POINT ( 'NONE',  ( -13.59724543428031573, -4.619798703722008959, 26.93261199819786356 ) ) ;
#8167 = CARTESIAN_POINT ( 'NONE',  ( -1.727091770866549414, -10.90442828429184274, 7.950000000000040146 ) ) ;
#8168 = CARTESIAN_POINT ( 'NONE',  ( 8.841785722321695573, -13.82664651025757152, 41.21024514465928235 ) ) ;
#8169 = ORIENTED_EDGE ( 'NONE', *, *, #3340, .F. ) ;
#8170 = CARTESIAN_POINT ( 'NONE',  ( -13.20632197976503086, 7.391146522708670119, 48.73000000000002530 ) ) ;
#8171 = SHAPE_REPRESENTATION ( 'socket head cap screw_iso_ISO 4762 M4 x 10 - 10N', ( #3995 ), #2439 ) ;
#8172 = CARTESIAN_POINT ( 'NONE',  ( 5.420364854932001819, 15.49051278174644430, 19.07142857142856940 ) ) ;
#8173 = CARTESIAN_POINT ( 'NONE',  ( 8.404922754268618235, 13.61519076058357491, 9.281673716087846415 ) ) ;
#8174 = DIRECTION ( 'NONE',  ( 0.000000000000000000, 0.000000000000000000, 1.000000000000000000 ) ) ;
#8175 = LINE ( 'NONE', #8863, #7764 ) ;
#8176 = CARTESIAN_POINT ( 'NONE',  ( -4.355403765523468529, -8.442910196168346815, 1.101137918078559208 ) ) ;
#8177 = CARTESIAN_POINT ( 'NONE',  ( 1.612135949262739398, 9.858066664633913234, -0.5488620819214271584 ) ) ;
#8178 = CARTESIAN_POINT ( 'NONE',  ( -162.9191712434781039, 0.5589657928192890424, 14.99021695762547424 ) ) ;
#8179 = CARTESIAN_POINT ( 'NONE',  ( -8.621071003556675549, 13.96533075980314642, 34.21832628391215536 ) ) ;
#8180 = CARTESIAN_POINT ( 'NONE',  ( -4.623906867372410190, 13.21436662431711895, 36.42857142857143060 ) ) ;
#8181 = ADVANCED_FACE ( 'NONE', ( #5996 ), #9175, .F. ) ;
#8182 = CARTESIAN_POINT ( 'NONE',  ( -4.623906867372410190, 13.21436662431711895, 36.42857142857143060 ) ) ;
#8183 = ORIENTED_EDGE ( 'NONE', *, *, #4530, .F. ) ;
#8184 = CARTESIAN_POINT ( 'NONE',  ( 5.420364854932001819, 15.49051278174644430, 49.07142857142859071 ) ) ;
#8185 = DIRECTION ( 'NONE',  ( 0.000000000000000000, -6.338944243255235518E-49, 1.000000000000000000 ) ) ;
#8186 = CARTESIAN_POINT ( 'NONE',  ( 1.837501619626330074, -16.30827793483733501, 9.642857142857147679 ) ) ;
#8187 = DIRECTION ( 'NONE',  ( 0.000000000000000000, 0.000000000000000000, 1.000000000000000000 ) ) ;
#8188 = CARTESIAN_POINT ( 'NONE',  ( -8.922933199037192509, 4.490180821391425603, 15.84886208192146739 ) ) ;
#8189 = CARTESIAN_POINT ( 'NONE',  ( -9.390499931835536884, 1.439022436064298249, 9.698862081921454603 ) ) ;
#8190 = CARTESIAN_POINT ( 'NONE',  ( 16.29368510291089223, -1.967016585148476882, 6.361183426769297711 ) ) ;
#8191 = CARTESIAN_POINT ( 'NONE',  ( 11.60466159355862104, 11.60466159355875071, 25.50000000000000711 ) ) ;
#8192 = ADVANCED_FACE ( 'NONE', ( #8384, #2851 ), #9892, .T. ) ;
#8193 = CARTESIAN_POINT ( 'NONE',  ( -8.620103694221995738, -13.47998361472161299, 8.289754855340721207 ) ) ;
#8194 = CARTESIAN_POINT ( 'NONE',  ( -13.55419868402807992, -4.742819248065651472, 16.92857142857143771 ) ) ;
#8195 = CARTESIAN_POINT ( 'NONE',  ( 0.000000000000000000, 0.000000000000000000, -1.270000000000007123 ) ) ;
#8196 = CARTESIAN_POINT ( 'NONE',  ( -1.677562661911643938, -10.91227292449344688, 8.948862081921467038 ) ) ;
#8197 = ORIENTED_EDGE ( 'NONE', *, *, #3066, .F. ) ;
#8198 = CARTESIAN_POINT ( 'NONE',  ( -11.85413878919593422, -7.448449071214776396, 22.71428571428571530 ) ) ;
#8199 = ORIENTED_EDGE ( 'NONE', *, *, #2781, .T. ) ;
#8200 = AXIS2_PLACEMENT_3D ( 'NONE', #6596, #9002, #6690 ) ;
#8201 = CARTESIAN_POINT ( 'NONE',  ( -11.60466159355861748, -11.60466159355874893, 34.50000000000000000 ) ) ;
#8202 = CARTESIAN_POINT ( 'NONE',  ( -8.841785722321695573, 13.82664651025757152, 50.21024514465927524 ) ) ;
#8203 = CARTESIAN_POINT ( 'NONE',  ( 7.424621202458790314, -7.424621202458697944, 10.50000000000000888 ) ) ;
#8204 = CARTESIAN_POINT ( 'NONE',  ( -10.15407889436378852, -10.15407889436390398, 10.50000000000000355 ) ) ;
#8205 = VERTEX_POINT ( 'NONE', #7457 ) ;
#8206 = CARTESIAN_POINT ( 'NONE',  ( 13.25633410266679313, -4.503970704919842305, 28.56738800180213644 ) ) ;
#8207 = COLOUR_RGB ( '', 0.66274510, 0.83137255, 0.94901961) ;
#8208 = FILL_AREA_STYLE_COLOUR ( '', #1441 ) ;
#8209 = CARTESIAN_POINT ( 'NONE',  ( -11.48991645990274257, -11.34085470199651979, -1.270000000000007123 ) ) ;
#8210 = EDGE_CURVE ( 'NONE', #7104, #8355, #8974, .T. ) ;
#8211 = CARTESIAN_POINT ( 'NONE',  ( 11.78653521626494793, 7.556039541191463371, 39.71024514465927524 ) ) ;
#8212 = CARTESIAN_POINT ( 'NONE',  ( -9.814260835641038128, 5.056896391392219137, 10.85113791807856209 ) ) ;
#8213 = CARTESIAN_POINT ( 'NONE',  ( 1.776620879821457333, 10.89658364409028124, 2.451137918078564848 ) ) ;
#8214 = CARTESIAN_POINT ( 'NONE',  ( 12.15899005565164792, -7.639999817571655250, 2.785714285714284255 ) ) ;
#8215 = FACE_OUTER_BOUND ( 'NONE', #9780, .T. ) ;
#8216 = CARTESIAN_POINT ( 'NONE',  ( -1.693770420379220099, -13.89774397934251837, 19.86118342676929416 ) ) ;
#8217 = SHAPE_REPRESENTATION_RELATIONSHIP ( 'NONE' , 'NONE' ,  #10217, #3629 ) ;
#8218 = PRODUCT_DEFINITION_SHAPE ( 'NONE', 'NONE',  #8652 ) ;
#8219 = CARTESIAN_POINT ( 'NONE',  ( 4.865839792409144771, 13.51115193377589740, 29.07546914105501301 ) ) ;
#8220 = CARTESIAN_POINT ( 'NONE',  ( 7.424621202458790314, -7.424621202458697944, 10.50000000000000888 ) ) ;
#8221 = CARTESIAN_POINT ( 'NONE',  ( -8.404922754268618235, -13.61519076058357491, 42.28167371608785174 ) ) ;
#8222 = CARTESIAN_POINT ( 'NONE',  ( -12.22926675870659174, 9.593933423190343035, 48.73000000000001819 ) ) ;
#8223 = CARTESIAN_POINT ( 'NONE',  ( 8.731428362939190890, -13.89598863503036164, 21.21428571428571885 ) ) ;
#8224 = CARTESIAN_POINT ( 'NONE',  ( -13.96533075980324234, 8.621071003556515677, 13.78167371608785174 ) ) ;
#8225 = CARTESIAN_POINT ( 'NONE',  ( -68.00000000000001421, 0.000000000000000000, 0.000000000000000000 ) ) ;
#8226 = CARTESIAN_POINT ( 'NONE',  ( 9.375578539472099848, -1.533232399699986370, 6.201137918078538647 ) ) ;
#8227 = CARTESIAN_POINT ( 'NONE',  ( 8.464561979789474222, 4.312909747525755400, 15.90000000000002522 ) ) ;
#8228 = CARTESIAN_POINT ( 'NONE',  ( -165.2816655742341823, 2.149895177073305685, 14.84513222368812002 ) ) ;
#8229 =( REPRESENTATION_RELATIONSHIP ('NONE','NONE', #58, #10217 ) REPRESENTATION_RELATIONSHIP_WITH_TRANSFORMATION ( #4646 )SHAPE_REPRESENTATION_RELATIONSHIP( ) );
#8230 = CARTESIAN_POINT ( 'NONE',  ( -11.69682198916834892, -11.51250119794901394, 38.50404056962644006 ) ) ;
#8231 = CARTESIAN_POINT ( 'NONE',  ( -13.55419868402807992, -4.742819248065651472, 28.92857142857143771 ) ) ;
#8232 = CARTESIAN_POINT ( 'NONE',  ( -7.448449071214644945, -11.85413878919601771, 40.28571428571428470 ) ) ;
#8233 = ORIENTED_EDGE ( 'NONE', *, *, #2812, .T. ) ;
#8234 = CARTESIAN_POINT ( 'NONE',  ( 5.297344310588354865, 15.53355953199867301, 3.067388001802140884 ) ) ;
#8235 = CYLINDRICAL_SURFACE ( 'NONE', #2802, 20.00000000000000000 ) ;
#8236 = CARTESIAN_POINT ( 'NONE',  ( -15.89939535829186923, -1.791431617653016062, 11.14285714285714235 ) ) ;
#8237 = DIRECTION ( 'NONE',  ( 1.000000000000000000, 4.755747939841215952E-17, -0.000000000000000000 ) ) ;
#8238 = CARTESIAN_POINT ( 'NONE',  ( -8.442910196168309511, -4.355403765523546689, 15.39886208192141126 ) ) ;
#8239 = CARTESIAN_POINT ( 'NONE',  ( 9.390499931835536884, -1.439022436064272270, 11.19886208192145816 ) ) ;
#8240 = UNCERTAINTY_MEASURE_WITH_UNIT (LENGTH_MEASURE( 1.000000000000000082E-05 ), #3266, 'distance_accuracy_value', 'NONE');
#8241 = CARTESIAN_POINT ( 'NONE',  ( 1.917699372585825790, 15.88516839912900203, 16.86118342676929061 ) ) ;
#8242 = CARTESIAN_POINT ( 'NONE',  ( -15.89939535829186923, -1.791431617653016062, 35.14285714285713880 ) ) ;
#8243 = EDGE_CURVE ( 'NONE', #6156, #7104, #7194, .T. ) ;
#8244 =( NAMED_UNIT ( * ) PLANE_ANGLE_UNIT ( ) SI_UNIT ( $, .RADIAN. ) );
#8245 = CARTESIAN_POINT ( 'NONE',  ( 8.621071003556677326, -13.96533075980314287, 7.218326283912148256 ) ) ;
#8246 = CARTESIAN_POINT ( 'NONE',  ( -7.448449071214644945, -11.85413878919601771, 22.28571428571428470 ) ) ;
#8247 = CARTESIAN_POINT ( 'NONE',  ( -15.10213328493390961, 5.284464991282586510, 11.57142857142857295 ) ) ;
#8248 = DIRECTION ( 'NONE',  ( 6.162975822039153635E-32, 0.5000000000000011102, 0.8660254037844379305 ) ) ;
#8249 = VERTEX_POINT ( 'NONE', #5136 ) ;
#8250 = CARTESIAN_POINT ( 'NONE',  ( 13.91197093850538380, 1.567502665446386390, 20.14285714285714235 ) ) ;
#8251 = ORIENTED_EDGE ( 'NONE', *, *, #3509, .F. ) ;
#8252 = CARTESIAN_POINT ( 'NONE',  ( -11.31370849898482156, 11.31370849898469544, 36.00000000000000711 ) ) ;
#8253 = CIRCLE ( 'NONE', #9254, 6.999999999999999112 ) ;
#8254 = AXIS2_PLACEMENT_3D ( 'NONE', #8283, #4410, #1206 ) ;
#8255 = CARTESIAN_POINT ( 'NONE',  ( 15.88516839912898071, 1.917699372586004092, 46.13881657323070584 ) ) ;
#8256 = CARTESIAN_POINT ( 'NONE',  ( -7.806708723663830618, -7.806708723663901672, 17.25000000000003553 ) ) ;
#8257 = SHAPE_DEFINITION_REPRESENTATION ( #6552, #10217 ) ;
#8258 = CARTESIAN_POINT ( 'NONE',  ( -13.21436662431716869, 4.623906867372262752, 17.57142857142856940 ) ) ;
#8259 = EDGE_CURVE ( 'NONE', #7029, #2493, #6748, .T. ) ;
#8260 = VECTOR ( 'NONE', #3126, 1000.000000000000000 ) ;
#8261 = CIRCLE ( 'NONE', #9760, 2.200000000000001066 ) ;
#8262 = VECTOR ( 'NONE', #2379, 1000.000000000000114 ) ;
#8263 = CARTESIAN_POINT ( 'NONE',  ( -13.89774397934249706, -1.693770420379375974, 25.13881657323070939 ) ) ;
#8264 = ORIENTED_EDGE ( 'NONE', *, *, #1932, .F. ) ;
#8265 = CARTESIAN_POINT ( 'NONE',  ( -166.6391998862286243, 0.2171903991958598068, 12.99861672450135330 ) ) ;
#8266 = CARTESIAN_POINT ( 'NONE',  ( 7.027753727702739539, 7.098671581784282480, 4.748862081921425116 ) ) ;
#8267 = CARTESIAN_POINT ( 'NONE',  ( 13.91197093850538380, 1.567502665446386390, 2.142857142857140573 ) ) ;
#8268 = CARTESIAN_POINT ( 'NONE',  ( -5.012215536711506658, 9.837026868206027785, 3.149999999999957723 ) ) ;
#8270 = AXIS2_PLACEMENT_3D ( 'NONE', #9490, #10047, #1425 ) ;
#8269 = CARTESIAN_POINT ( 'NONE',  ( -9.814260835641038128, 5.056896391392221801, 4.851137918078532785 ) ) ;
#8271 = DIRECTION ( 'NONE',  ( 1.000000000000000000, 4.755747939841215952E-17, -0.000000000000000000 ) ) ;
#8272 = CARTESIAN_POINT ( 'NONE',  ( -13.17239914596754424, 4.743843029824683200, 33.57546914105500946 ) ) ;
#8273 =( NAMED_UNIT ( * ) SI_UNIT ( $, .STERADIAN. ) SOLID_ANGLE_UNIT ( ) );
#8274 = CARTESIAN_POINT ( 'NONE',  ( -1.693770420379220099, -13.89774397934251837, 19.86118342676929416 ) ) ;
#8275 = CARTESIAN_POINT ( 'NONE',  ( -10.90442828429183919, -1.727091770866655329, 5.549999999999999822 ) ) ;
#8276 = CARTESIAN_POINT ( 'NONE',  ( 5.404401153735178376, -15.06016580658422477, 35.42453085894499765 ) ) ;
#8277 = CARTESIAN_POINT ( 'NONE',  ( -9.891020467832197127, 12.31459401221520800, 48.72999999999998977 ) ) ;
#8278 = CARTESIAN_POINT ( 'NONE',  ( -13.89598863503046111, 8.731428362939027465, 17.78571428571428115 ) ) ;
#8279 = CARTESIAN_POINT ( 'NONE',  ( -58.00000000000002132, 7.703719777548943412E-30, -1.059261469412979719E-30 ) ) ;
#8280 = CARTESIAN_POINT ( 'NONE',  ( 7.340858601237956194, 11.92174236212700045, 15.28167371608785174 ) ) ;
#8281 = CARTESIAN_POINT ( 'NONE',  ( -9.375578539472099848, 1.533232399700010351, 7.701137918078540423 ) ) ;
#8282 = CARTESIAN_POINT ( 'NONE',  ( -8.900167166472156666, 4.534861676072234893, 17.85000000000001918 ) ) ;
#8283 = CARTESIAN_POINT ( 'NONE',  ( 0.000000000000000000, 0.000000000000000000, -1.270000000000007123 ) ) ;
#8284 = CARTESIAN_POINT ( 'NONE',  ( -1.707986654103994528, 16.32287076676380266, 34.64689771248358596 ) ) ;
#8285 = CARTESIAN_POINT ( 'NONE',  ( -7.639999817571787588, 12.15899005565156266, 30.21428571428572596 ) ) ;
#8286 = PRODUCT_DEFINITION_SHAPE ( 'NONE', 'NONE',  #10236 ) ;
#8287 = CARTESIAN_POINT ( 'NONE',  ( -4.742819248065502258, -13.55419868402813677, 40.07142857142857650 ) ) ;
#8288 = ORIENTED_EDGE ( 'NONE', *, *, #8067, .T. ) ;
#8289 = CARTESIAN_POINT ( 'NONE',  ( 11.31370849898482334, -11.31370849898469366, 45.00000000000000711 ) ) ;
#8290 = CARTESIAN_POINT ( 'NONE',  ( -88.00000000000002842, 0.000000000000000000, 8.000000000000000000 ) ) ;
#8291 = CARTESIAN_POINT ( 'NONE',  ( 15.10213328493390783, -5.284464991282587398, 14.57142857142856940 ) ) ;
#8292 = DIRECTION ( 'NONE',  ( -1.000000000000000000, 1.842239752758738928E-31, -1.780435181894459419E-32 ) ) ;
#8293 = FILL_AREA_STYLE_COLOUR ( '', #2175 ) ;
#8294 = EDGE_CURVE ( 'NONE', #6875, #4862, #3971, .T. ) ;
#8295 = DIRECTION ( 'NONE',  ( -1.000000000000000000, -0.000000000000000000, -0.000000000000000000 ) ) ;
#8296 = CARTESIAN_POINT ( 'NONE',  ( 9.390499931835536884, -1.439022436064273158, 20.19886208192146526 ) ) ;
#8297 = CARTESIAN_POINT ( 'NONE',  ( -6.751237864895158758, 6.683790977649261222, 6.998862081921422451 ) ) ;
#8298 = CARTESIAN_POINT ( 'NONE',  ( -5.012215536711506658, 9.837026868206027785, 12.14999999999996305 ) ) ;
#8299 = CARTESIAN_POINT ( 'NONE',  ( 15.91362231745475597, 1.665163862720026255, 6.146897712483580634 ) ) ;
#8300 = CARTESIAN_POINT ( 'NONE',  ( 5.284464991282756152, -15.10213328493384743, 27.42857142857143060 ) ) ;
#8301 = DIRECTION ( 'NONE',  ( -4.755747939841215952E-17, 1.000000000000000000, 0.000000000000000000 ) ) ;
#8302 = CARTESIAN_POINT ( 'NONE',  ( 16.29368510291089223, -1.967016585148476882, 6.361183426769297711 ) ) ;
#8303 = AXIS2_PLACEMENT_3D ( 'NONE', #9990, #2791, #5939 ) ;
#8304 = CARTESIAN_POINT ( 'NONE',  ( 4.623906867372411078, -13.21436662431711717, 21.42857142857142705 ) ) ;
#8305 = CARTESIAN_POINT ( 'NONE',  ( 8.512513224245308763, 13.54758718765259040, 1.285714285714285809 ) ) ;
#8306 = CARTESIAN_POINT ( 'NONE',  ( -15.10213328493390961, 5.284464991282586510, 47.57142857142857650 ) ) ;
#8307 = VERTEX_POINT ( 'NONE', #1885 ) ;
#8308 = CARTESIAN_POINT ( 'NONE',  ( -13.91197093850538380, -1.567502665446387278, 11.14285714285714235 ) ) ;
#8309 = ORIENTED_EDGE ( 'NONE', *, *, #1508, .F. ) ;
#8310 = CARTESIAN_POINT ( 'NONE',  ( 8.731428362939189114, -13.89598863503035986, 27.21428571428571885 ) ) ;
#8311 = ADVANCED_FACE ( 'NONE', ( #5033 ), #331, .F. ) ;
#8312 = CARTESIAN_POINT ( 'NONE',  ( 13.89774397934249706, 1.693770420379375308, 4.138816573230708507 ) ) ;
#8313 = CARTESIAN_POINT ( 'NONE',  ( 9.837026868206066865, -5.012215536711395636, 16.35000000000000497 ) ) ;
#8314 = PRODUCT_DEFINITION_SHAPE ( 'NONE', 'NONE',  #6036 ) ;
#8315 = APPLICATION_PROTOCOL_DEFINITION ( 'draft international standard', 'automotive_design', 1998, #5533 ) ;
#8316 = CARTESIAN_POINT ( 'NONE',  ( -12.15899005565164792, 7.639999817571650809, 17.78571428571428825 ) ) ;
#8317 = CARTESIAN_POINT ( 'NONE',  ( -9.989344678689363377, 9.809645194533960222, 25.99595943037356349 ) ) ;
#8318 = ORIENTED_EDGE ( 'NONE', *, *, #10088, .F. ) ;
#8319 = DIRECTION ( 'NONE',  ( -1.000000000000000000, 1.842239752758738928E-31, -1.780435181894459419E-32 ) ) ;
#8320 = FACE_OUTER_BOUND ( 'NONE', #4360, .T. ) ;
#8321 = CARTESIAN_POINT ( 'NONE',  ( 7.458344646081711105, -7.390897758835786036, 20.49886208192143400 ) ) ;
#8322 = CARTESIAN_POINT ( 'NONE',  ( -13.25633410266679313, 4.503970704919840529, 49.56738800180214355 ) ) ;
#8323 = CARTESIAN_POINT ( 'NONE',  ( 1.642561882922480621, -10.37072757624891750, 7.800000000000029132 ) ) ;
#8324 = CARTESIAN_POINT ( 'NONE',  ( 1.595456901104624459, -10.37818827243065201, 3.801137918078595135 ) ) ;
#8325 = DIRECTION ( 'NONE',  ( 1.000000000000000000, 0.000000000000000000, 0.000000000000000000 ) ) ;
#8326 = CARTESIAN_POINT ( 'NONE',  ( -13.59724543428031573, -4.619798703722008959, 32.93261199819787777 ) ) ;
#8327 = CARTESIAN_POINT ( 'NONE',  ( -7.424621202458789426, 7.424621202458720148, 3.000000000000002665 ) ) ;
#8328 = CARTESIAN_POINT ( 'NONE',  ( 13.47998361472151529, 8.620103694222146729, 45.71024514465928235 ) ) ;
#8329 = CARTESIAN_POINT ( 'NONE',  ( -13.20330265076414911, 7.287341860736131771, 48.72999999999998977 ) ) ;
#8330 = DIRECTION ( 'NONE',  ( 0.000000000000000000, 6.938893903907220674E-18, 1.000000000000000000 ) ) ;
#8331 = CARTESIAN_POINT ( 'NONE',  ( 9.989344678689365153, -9.809645194533958446, 10.99595943037356882 ) ) ;
#8332 = CARTESIAN_POINT ( 'NONE',  ( 6.683790977649321619, -6.751237864895082375, 12.50113791807859265 ) ) ;
#8333 = CARTESIAN_POINT ( 'NONE',  ( -6.717514421272238856, 6.717514421272180236, 15.00000000000001421 ) ) ;
#8334 = CARTESIAN_POINT ( 'NONE',  ( -166.3218336876412593, 1.718641102943201604, 14.90254673046750433 ) ) ;
#8335 = CARTESIAN_POINT ( 'NONE',  ( 12.15899005565164792, -7.639999817571655250, 38.78571428571429180 ) ) ;
#8336 = CARTESIAN_POINT ( 'NONE',  ( 7.448449071214646722, 11.85413878919601594, 37.28571428571429180 ) ) ;
#8337 = VERTEX_POINT ( 'NONE', #6708 ) ;
#8338 = CARTESIAN_POINT ( 'NONE',  ( 1.791431617652837316, 15.89939535829188877, 48.85714285714286120 ) ) ;
#8339 = CARTESIAN_POINT ( 'NONE',  ( -3.974304365018271223, 15.37125927611797493, 1.442806492371165318E-14 ) ) ;
#8340 = CARTESIAN_POINT ( 'NONE',  ( 13.89598863503046111, -8.731428362939032795, 26.78571428571429536 ) ) ;
#8341 = DIRECTION ( 'NONE',  ( 1.000000000000000000, 0.000000000000000000, 0.000000000000000000 ) ) ;
#8342 = CARTESIAN_POINT ( 'NONE',  ( -70.00000000000001421, 0.000000000000000000, 0.000000000000000000 ) ) ;
#8343 = CARTESIAN_POINT ( 'NONE',  ( 2.000000000000001776, 1.773042676681366281, 0.000000000000000000 ) ) ;
#8344 = CARTESIAN_POINT ( 'NONE',  ( 9.865911304835474738, 1.562606840307949829, 7.050000000000010481 ) ) ;
#8345 = CARTESIAN_POINT ( 'NONE',  ( 4.270415729527831772, 8.486213763410688671, 4.598862081921435419 ) ) ;
#8346 = PRODUCT_DEFINITION_CONTEXT ( 'detailed design', #9444, 'design' ) ;
#8347 = CARTESIAN_POINT ( 'NONE',  ( 10.90442828429183919, 1.727091770866679532, 16.04999999999995808 ) ) ;
#8348 = EDGE_CURVE ( 'NONE', #7728, #1810, #8929, .T. ) ;
#8349 = CARTESIAN_POINT ( 'NONE',  ( 13.61519076058348254, 8.404922754268771001, 11.71832628391215181 ) ) ;
#8350 = CARTESIAN_POINT ( 'NONE',  ( -1.791431617652833763, -15.89939535829188877, 39.85714285714286120 ) ) ;
#8351 = CARTESIAN_POINT ( 'NONE',  ( 13.61519076058348254, 8.404922754268771001, -0.2816737160878517443 ) ) ;
#8352 = CARTESIAN_POINT ( 'NONE',  ( 13.55419868402807992, 4.742819248065648807, 19.92857142857143771 ) ) ;
#8353 = CARTESIAN_POINT ( 'NONE',  ( 11.60466159355862104, 11.60466159355875071, 1.500000000000003553 ) ) ;
#8354 = CARTESIAN_POINT ( 'NONE',  ( -8.731428362939189114, 13.89598863503036341, 48.21428571428570820 ) ) ;
#8355 = VERTEX_POINT ( 'NONE', #9994 ) ;
#8356 = CARTESIAN_POINT ( 'NONE',  ( 7.806708723663831506, 7.806708723663931870, 18.74999999999998934 ) ) ;
#8357 = ORIENTED_EDGE ( 'NONE', *, *, #6836, .T. ) ;
#8358 = CARTESIAN_POINT ( 'NONE',  ( -5.284464991282755264, 15.10213328493384743, 30.42857142857143060 ) ) ;
#8359 = CARTESIAN_POINT ( 'NONE',  ( 10.06191849875406064, 10.24623928997363187, 3.495959430373559940 ) ) ;
#8360 = CARTESIAN_POINT ( 'NONE',  ( 1.689666864740335894, -10.36326688006721497, 2.798862081921426714 ) ) ;
#8361 = PRODUCT_CONTEXT ( 'NONE', #8904, 'mechanical' ) ;
#8362 = CARTESIAN_POINT ( 'NONE',  ( -7.639999817571786700, 12.15899005565156266, 30.21428571428572241 ) ) ;
#8363 = CARTESIAN_POINT ( 'NONE',  ( 9.989344678689365153, -9.809645194533958446, 22.99595943037356705 ) ) ;
#8364 = ORIENTED_EDGE ( 'NONE', *, *, #2781, .F. ) ;
#8365 = CARTESIAN_POINT ( 'NONE',  ( -1.642561882922479732, 10.37072757624895303, 18.29999999999998295 ) ) ;
#8366 = CARTESIAN_POINT ( 'NONE',  ( -70.00000000000001421, 0.000000000000000000, 8.500000000000000000 ) ) ;
#8367 = APPLICATION_CONTEXT ( 'automotive_design' ) ;
#8368 = EDGE_CURVE ( 'NONE', #8072, #2212, #2154, .T. ) ;
#8369 = CARTESIAN_POINT ( 'NONE',  ( 6.751237864895159646, -6.683790977649239906, 2.498862081921459755 ) ) ;
#8370 = CARTESIAN_POINT ( 'NONE',  ( -5.012215536711506658, 9.837026868206022456, 6.149999999999980815 ) ) ;
#8371 = CARTESIAN_POINT ( 'NONE',  ( -1.776620879821455556, -10.89658364409025637, 12.95113791807858128 ) ) ;
#8372 = AXIS2_PLACEMENT_3D ( 'NONE', #5719, #8733, #7067 ) ;
#8373 = LINE ( 'NONE', #3673, #5784 ) ;
#8374 = CARTESIAN_POINT ( 'NONE',  ( 13.17239914596754424, -4.743843029824685864, 24.57546914105500946 ) ) ;
#8375 = FILL_AREA_STYLE ('',( #5787 ) ) ;
#8376 = CARTESIAN_POINT ( 'NONE',  ( 7.424621202458790314, -7.424621202458697944, 7.500000000000007105 ) ) ;
#8377 = CARTESIAN_POINT ( 'NONE',  ( 13.96533075980324234, -8.621071003556521006, 34.78167371608785885 ) ) ;
#8378 = CARTESIAN_POINT ( 'NONE',  ( -13.10821530951307778, 7.834963172504977535, 48.73000000000001108 ) ) ;
#8379 = CARTESIAN_POINT ( 'NONE',  ( 16.00000000000000000, 1.959434878635765131E-15, 113.2548339959390518 ) ) ;
#8380 = CARTESIAN_POINT ( 'NONE',  ( -1.737328882695368115, 14.25515036105620581, 20.63881657323070939 ) ) ;
#8381 = CARTESIAN_POINT ( 'NONE',  ( 9.873755945037075321, 1.513077731353044131, 18.05113791807859513 ) ) ;
#8382 = CARTESIAN_POINT ( 'NONE',  ( 1.439022436064387511, -9.390499931835510239, 6.801137918078597799 ) ) ;
#8383 = EDGE_CURVE ( 'NONE', #7869, #503, #1006, .T. ) ;
#8384 = FACE_BOUND ( 'NONE', #8850, .T. ) ;
#8385 = CARTESIAN_POINT ( 'NONE',  ( -11.85413878919593422, -7.448449071214776396, 40.71428571428571530 ) ) ;
#8386 = CARTESIAN_POINT ( 'NONE',  ( -13.92619789766827054, -1.441234910513399470, 3.146897712483577969 ) ) ;
#8387 = ORIENTED_EDGE ( 'NONE', *, *, #74, .T. ) ;
#8388 = CARTESIAN_POINT ( 'NONE',  ( 13.54758718765249803, 8.512513224245457977, 43.71428571428572241 ) ) ;
#8389 = CARTESIAN_POINT ( 'NONE',  ( -1.045875314801341771, 15.69722212429930330, -1.227588689168360484E-16 ) ) ;
#8390 = CARTESIAN_POINT ( 'NONE',  ( -15.89939535829186923, -1.791431617653016062, 35.14285714285713880 ) ) ;
#8391 = DIRECTION ( 'NONE',  ( 1.000000000000000000, 0.000000000000000000, 0.000000000000000000 ) ) ;
#8392 = CARTESIAN_POINT ( 'NONE',  ( 2.000000000000001776, 1.773042676681366281, 0.000000000000000000 ) ) ;
#8393 = CARTESIAN_POINT ( 'NONE',  ( 8.900167166472154889, -4.534861676072210912, 7.350000000000000533 ) ) ;
#8394 = CARTESIAN_POINT ( 'NONE',  ( -4.270415729527831772, -8.486213763410678013, 3.098862081921434974 ) ) ;
#8395 = CARTESIAN_POINT ( 'NONE',  ( 10.37072757624895836, -1.642561882922355609, 10.19999999999998685 ) ) ;
#8396 = CARTESIAN_POINT ( 'NONE',  ( 15.10213328493390783, -5.284464991282587398, 38.57142857142857650 ) ) ;
#8397 =( LENGTH_UNIT ( ) NAMED_UNIT ( * ) SI_UNIT ( .MILLI., .METRE. ) );
#8398 = CARTESIAN_POINT ( 'NONE',  ( 8.621071003556677326, -13.96533075980314287, 25.21832628391215181 ) ) ;
#8399 = CARTESIAN_POINT ( 'NONE',  ( -4.742819248065502258, -13.55419868402813677, 22.07142857142858006 ) ) ;
#8400 = CARTESIAN_POINT ( 'NONE',  ( 1.791431617652837316, 15.89939535829188877, 0.8571428571428549859 ) ) ;
#8401 = CARTESIAN_POINT ( 'NONE',  ( 11.60466159355862104, 11.60466159355875071, 43.50000000000000711 ) ) ;
#8402 = EDGE_LOOP ( 'NONE', ( #154, #1553, #2800, #2991 ) ) ;
#8403 = CARTESIAN_POINT ( 'NONE',  ( 10.90442828429183919, 1.727091770866679532, 16.04999999999995808 ) ) ;
#8404 = ADVANCED_FACE ( 'NONE', ( #2239 ), #7674, .F. ) ;
#8405 = EDGE_LOOP ( 'NONE', ( #3874, #3353, #6318, #3429 ) ) ;
#8406 = CARTESIAN_POINT ( 'NONE',  ( 11.60466159355861926, 11.60466159355874716, 43.50000000000000711 ) ) ;
#8407 = CARTESIAN_POINT ( 'NONE',  ( -11.78653521626494793, -7.556039541191465148, 6.710245144659284122 ) ) ;
#8408 = CARTESIAN_POINT ( 'NONE',  ( 4.766900247265192903, 9.355568503977902850, 15.60000000000000320 ) ) ;
#8409 = CARTESIAN_POINT ( 'NONE',  ( 15.89939535829187278, 1.791431617653015174, 2.142857142857140573 ) ) ;
#8410 = CIRCLE ( 'NONE', #7916, 13.00000000000001421 ) ;
#8411 = CARTESIAN_POINT ( 'NONE',  ( 15.49051278174638036, 5.420364854932175014, 7.928571428571430602 ) ) ;
#8412 = CARTESIAN_POINT ( 'NONE',  ( -7.448449071214644945, -11.85413878919601771, 22.28571428571428470 ) ) ;
#8413 = VERTEX_POINT ( 'NONE', #2953 ) ;
#8414 = CARTESIAN_POINT ( 'NONE',  ( -13.51115193377584589, -4.865839792409295761, 42.92453085894499054 ) ) ;
#8415 = AXIS2_PLACEMENT_3D ( 'NONE', #1457, #49, #7025 ) ;
#8416 = EDGE_LOOP ( 'NONE', ( #795, #676, #7079, #2619 ) ) ;
#8417 = CARTESIAN_POINT ( 'NONE',  ( -68.00000000000002842, 0.000000000000000000, 0.000000000000000000 ) ) ;
#8418 = CARTESIAN_POINT ( 'NONE',  ( 16.32287076676382043, -1.707986654103810897, 28.35310228751642825 ) ) ;
#8419 = AXIS2_PLACEMENT_3D ( 'NONE', #4108, #1631, #4009 ) ;
#8420 = CARTESIAN_POINT ( 'NONE',  ( 2.000000000000001776, -0.8865213383406761460, 1.535499999999911935 ) ) ;
#8421 = CARTESIAN_POINT ( 'NONE',  ( 7.771249796623105333, 7.842167650704658932, 16.74886208192143755 ) ) ;
#8422 = CARTESIAN_POINT ( 'NONE',  ( 10.37072757624895836, -1.642561882922355609, 10.19999999999998685 ) ) ;
#8423 = CARTESIAN_POINT ( 'NONE',  ( -7.390897758835869524, 7.458344646081644491, 17.00113791807859442 ) ) ;
#8424 = DIRECTION ( 'NONE',  ( 1.000000000000000000, -4.575525868300071581E-16, -0.000000000000000000 ) ) ;
#8425 = AXIS2_PLACEMENT_3D ( 'NONE', #3798, #4623, #4725 ) ;
#8426 = COLOUR_RGB ( '', 0.72549020, 0.75294118, 0.79215686) ;
#8427 = VECTOR ( 'NONE', #4768, 1000.000000000000000 ) ;
#8428 =( NAMED_UNIT ( * ) SI_UNIT ( $, .STERADIAN. ) SOLID_ANGLE_UNIT ( ) );
#8429 = CARTESIAN_POINT ( 'NONE',  ( -4.724406229267374968, -9.377220287599046245, 3.098862081921434974 ) ) ;
#8430 = CARTESIAN_POINT ( 'NONE',  ( 1.967016585148662289, -16.29368510291087091, 47.63881657323071295 ) ) ;
#8431 = CARTESIAN_POINT ( 'NONE',  ( 9.837026868206070418, -5.012215536711392083, 1.350000000000015410 ) ) ;
#8432 = CARTESIAN_POINT ( 'NONE',  ( -5.420364854931999155, -15.49051278174644253, 28.07142857142857295 ) ) ;
#8433 = DIRECTION ( 'NONE',  ( 1.000000000000000000, 0.000000000000000000, 0.000000000000000000 ) ) ;
#8434 = CIRCLE ( 'NONE', #9273, 8.000000000000000000 ) ;
#8435 = CIRCLE ( 'NONE', #4782, 18.00000000000000355 ) ;
#8436 = TOROIDAL_SURFACE ( 'NONE', #6443, 8.000000000000000000, 1.000000000000000888 ) ;
#8437 = CARTESIAN_POINT ( 'NONE',  ( -4.743843029824828861, 13.17239914596749450, 20.42453085894499054 ) ) ;
#8438 = CARTESIAN_POINT ( 'NONE',  ( 1.776620879821457333, 10.89658364409028124, -0.5488620819214271584 ) ) ;
#8439 = CARTESIAN_POINT ( 'NONE',  ( -4.490180821391513533, 8.922933199037158758, 2.151137918078574796 ) ) ;
#8440 = CARTESIAN_POINT ( 'NONE',  ( -163.6882088544006706, -1.709196472000179323, 12.88739062898286214 ) ) ;
#8441 = CARTESIAN_POINT ( 'NONE',  ( -10.15407889436378852, -10.15407889436390576, 40.50000000000000711 ) ) ;
#8442 = CARTESIAN_POINT ( 'NONE',  ( 13.59724543428031573, 4.619798703722006294, 5.932611998197868886 ) ) ;
#8443 = ORIENTED_EDGE ( 'NONE', *, *, #6843, .F. ) ;
#8444 = CARTESIAN_POINT ( 'NONE',  ( -16.32287076676382398, 1.707986654103809343, 7.353102287516419366 ) ) ;
#8445 = DIRECTION ( 'NONE',  ( -1.000000000000000000, -0.000000000000000000, -0.000000000000000000 ) ) ;
#8446 = CARTESIAN_POINT ( 'NONE',  ( 11.60466159355862104, 11.60466159355875071, 25.50000000000000711 ) ) ;
#8447 = CARTESIAN_POINT ( 'NONE',  ( 4.000000000000003553, 0.000000000000000000, 0.000000000000000000 ) ) ;
#8448 = FACE_OUTER_BOUND ( 'NONE', #662, .T. ) ;
#8449 = DIRECTION ( 'NONE',  ( -1.000000000000000000, -1.387778780781445676E-16, -0.000000000000000000 ) ) ;
#8450 = CARTESIAN_POINT ( 'NONE',  ( -4.534861676072319270, 8.900167166472121139, 3.149999999999957723 ) ) ;
#8451 = CARTESIAN_POINT ( 'NONE',  ( 4.270415729527831772, 8.486213763410697553, 16.59886208192144252 ) ) ;
#8452 = DIRECTION ( 'NONE',  ( 0.000000000000000000, 0.000000000000000000, 1.000000000000000000 ) ) ;
#8453 = VECTOR ( 'NONE', #1754, 1000.000000000000000 ) ;
#8454 = CARTESIAN_POINT ( 'NONE',  ( 5.420364854932001819, 15.49051278174644430, 49.07142857142859071 ) ) ;
#8455 = ADVANCED_BREP_SHAPE_REPRESENTATION ( '', ( #147, #3995 ), #6118 ) ;
#8456 = FILL_AREA_STYLE_COLOUR ( '', #1517 ) ;
#8457 = CARTESIAN_POINT ( 'NONE',  ( -1.707986654103994528, 16.32287076676380266, 16.64689771248358596 ) ) ;
#8458 = CARTESIAN_POINT ( 'NONE',  ( 1.567502665446232957, 13.91197093850540156, 30.85714285714286120 ) ) ;
#8459 = CARTESIAN_POINT ( 'NONE',  ( -8.512513224245306986, -13.54758718765259218, 4.285714285714288252 ) ) ;
#8460 = CARTESIAN_POINT ( 'NONE',  ( -1.791431617652833763, -15.89939535829188877, 45.85714285714286120 ) ) ;
#8461 = EDGE_LOOP ( 'NONE', ( #1760, #3963 ) ) ;
#8462 = CARTESIAN_POINT ( 'NONE',  ( 10.90442828429183919, 1.727091770866679532, 13.04999999999999538 ) ) ;
#8463 = FILL_AREA_STYLE_COLOUR ( '', #8952 ) ;
#8464 = CARTESIAN_POINT ( 'NONE',  ( -15.10213328493390961, 5.284464991282586510, 47.57142857142857650 ) ) ;
#8465 = DIRECTION ( 'NONE',  ( 0.000000000000000000, 0.000000000000000000, 1.000000000000000000 ) ) ;
#8466 = CARTESIAN_POINT ( 'NONE',  ( 10.06191849875406064, 10.24623928997363187, 9.495959430373563492 ) ) ;
#8467 = CARTESIAN_POINT ( 'NONE',  ( 10.37818827243067510, -1.595456901104499448, 2.198862081921450606 ) ) ;
#8468 = CARTESIAN_POINT ( 'NONE',  ( 11.60466159355862104, 11.60466159355875071, 1.500000000000003553 ) ) ;
#8469 = CARTESIAN_POINT ( 'NONE',  ( 13.54758718765249803, 8.512513224245457977, 1.714285714285716855 ) ) ;
#8470 = CIRCLE ( 'NONE', #8811, 15.44569104238500046 ) ;
#8471 = CARTESIAN_POINT ( 'NONE',  ( -11.85413878919593422, -7.448449071214776396, 22.71428571428571530 ) ) ;
#8472 = CARTESIAN_POINT ( 'NONE',  ( -10.24623928997352351, -10.06191849875416899, 20.50404056962644006 ) ) ;
#8473 = AXIS2_PLACEMENT_3D ( 'NONE', #6936, #6211, #7827 ) ;
#8474 = ORIENTED_EDGE ( 'NONE', *, *, #6023, .T. ) ;
#8475 = CARTESIAN_POINT ( 'NONE',  ( -4.743843029824828861, 13.17239914596749450, 38.42453085894499054 ) ) ;
#8476 = ORIENTED_EDGE ( 'NONE', *, *, #5748, .F. ) ;
#8477 = CARTESIAN_POINT ( 'NONE',  ( -13.96533075980324234, 8.621071003556515677, 25.78167371608785530 ) ) ;
#8478 = DIRECTION ( 'NONE',  ( 0.000000000000000000, 1.000000000000000000, -1.332267629550187849E-15 ) ) ;
#8479 = CARTESIAN_POINT ( 'NONE',  ( 1.533232399700100945, -9.375578539472073203, 2.798862081921426714 ) ) ;
#8480 = EDGE_CURVE ( 'NONE', #8072, #5915, #8596, .T. ) ;
#8481 = CARTESIAN_POINT ( 'NONE',  ( 7.448449071214646722, 11.85413878919601594, 1.285714285714285809 ) ) ;
#8482 = CARTESIAN_POINT ( 'NONE',  ( 7.424621202458790314, -7.424621202458697944, 4.500000000000003553 ) ) ;
#8483 = CARTESIAN_POINT ( 'NONE',  ( -5.012215536711506658, 9.837026868206027785, 0.1499999999999952482 ) ) ;
#8484 = FACE_OUTER_BOUND ( 'NONE', #2371, .T. ) ;
#8485 = CARTESIAN_POINT ( 'NONE',  ( -10.24623928997352351, -10.06191849875416899, 26.50404056962643651 ) ) ;
#8486 = EDGE_LOOP ( 'NONE', ( #6616, #6284, #625, #6689 ) ) ;
#8487 = CARTESIAN_POINT ( 'NONE',  ( 4.743843029824831525, -13.17239914596749095, 5.424530858944991429 ) ) ;
#8488 = CARTESIAN_POINT ( 'NONE',  ( -5.012215536711508435, 9.837026868206020680, 6.149999999999979927 ) ) ;
#8489 = CARTESIAN_POINT ( 'NONE',  ( -11.60466159355861926, -11.60466159355875249, 28.50000000000001066 ) ) ;
#8490 = DIRECTION ( 'NONE',  ( 1.000000000000000000, 4.755747939841215952E-17, -0.000000000000000000 ) ) ;
#8491 = CARTESIAN_POINT ( 'NONE',  ( 14.28433602490915000, -1.478298951650544479, 16.35310228751641759 ) ) ;
#8492 = CARTESIAN_POINT ( 'NONE',  ( 6.683790977649321619, -6.751237864895076157, 15.50113791807859620 ) ) ;
#8493 = CARTESIAN_POINT ( 'NONE',  ( -9.873755945037078874, -1.513077731353020594, 1.551137918078593803 ) ) ;
#8494 = DIRECTION ( 'NONE',  ( -1.000000000000000000, -1.387778780781445676E-16, -0.000000000000000000 ) ) ;
#8495 = CARTESIAN_POINT ( 'NONE',  ( 7.448449071214646722, 11.85413878919601594, 43.28571428571429180 ) ) ;
#8496 = CARTESIAN_POINT ( 'NONE',  ( -1.478298951650703019, 14.28433602490913579, -1.353102287516420921 ) ) ;
#8497 = ORIENTED_EDGE ( 'NONE', *, *, #4186, .F. ) ;
#8498 = CARTESIAN_POINT ( 'NONE',  ( -1.967016585148659846, 16.29368510291087091, 8.638816573230704066 ) ) ;
#8499 = FACE_OUTER_BOUND ( 'NONE', #8486, .T. ) ;
#8500 = CARTESIAN_POINT ( 'NONE',  ( -5.284464991282755264, 15.10213328493384743, 30.42857142857143060 ) ) ;
#8501 = DIRECTION ( 'NONE',  ( -4.575525868300071581E-16, -1.000000000000000000, 0.000000000000000000 ) ) ;
#8502 = DIRECTION ( 'NONE',  ( 0.000000000000000000, -8.191099868251446680E-34, -1.000000000000000000 ) ) ;
#8503 = CARTESIAN_POINT ( 'NONE',  ( -1.562606840307830591, -9.865911304835488949, 4.950000000000017053 ) ) ;
#8504 = CARTESIAN_POINT ( 'NONE',  ( -6.751237864895158758, 6.683790977649261222, 15.99886208192142512 ) ) ;
#8505 = EDGE_CURVE ( 'NONE', #928, #9861, #1985, .T. ) ;
#8506 = CARTESIAN_POINT ( 'NONE',  ( -158.0000000000000284, -7.514081744949122117E-15, 0.000000000000000000 ) ) ;
#8507 = CARTESIAN_POINT ( 'NONE',  ( 11.31370849898469899, 11.31370849898481978, 49.50000000000000711 ) ) ;
#8508 = SURFACE_SIDE_STYLE ('',( #1223 ) ) ;
#8509 = CARTESIAN_POINT ( 'NONE',  ( -16.29368510291090288, 1.967016585148476215, 21.36118342676929771 ) ) ;
#8510 = CARTESIAN_POINT ( 'NONE',  ( 5.284464991282756152, -15.10213328493384743, 21.42857142857142705 ) ) ;
#8511 = DIRECTION ( 'NONE',  ( -1.000000000000000000, -1.387778780781445676E-16, -0.000000000000000000 ) ) ;
#8512 = ORIENTED_EDGE ( 'NONE', *, *, #5747, .F. ) ;
#8513 = CARTESIAN_POINT ( 'NONE',  ( 14.00000000000000533, 1.609999999999986553, 5.551115123125782702E-14 ) ) ;
#8514 = VERTEX_POINT ( 'NONE', #6983 ) ;
#8515 = CARTESIAN_POINT ( 'NONE',  ( 15.89939535829187278, 1.791431617653015174, 44.14285714285714590 ) ) ;
#8516 = SHAPE_REPRESENTATION_RELATIONSHIP ( 'NONE' , 'NONE' ,  #3956, #939 ) ;
#8517 = EDGE_CURVE ( 'NONE', #8355, #1436, #4600, .T. ) ;
#8518 = CARTESIAN_POINT ( 'NONE',  ( -10.89658364409024749, -1.776620879821561472, 12.54886208192144004 ) ) ;
#8519 = CARTESIAN_POINT ( 'NONE',  ( 15.49051278174638036, 5.420364854932175014, 1.928571428571430380 ) ) ;
#8520 = CARTESIAN_POINT ( 'NONE',  ( -1.837501619626328297, 16.30827793483733856, 0.6428571428571432378 ) ) ;
#8521 = PRODUCT_RELATED_PRODUCT_CATEGORY ( 'part', '', ( #7484 ) ) ;
#8522 = CARTESIAN_POINT ( 'NONE',  ( 13.55419868402807992, 4.742819248065649695, 19.92857142857143415 ) ) ;
#8523 = CARTESIAN_POINT ( 'NONE',  ( 8.900167166472158442, -4.534861676072210024, 10.35000000000002274 ) ) ;
#8524 = CARTESIAN_POINT ( 'NONE',  ( -14.28433602490915000, 1.478298951650542481, 43.35310228751642825 ) ) ;
#8525 = ORIENTED_EDGE ( 'NONE', *, *, #268, .F. ) ;
#8526 = CARTESIAN_POINT ( 'NONE',  ( -165.0000000000000284, -1.734723475976807094E-15, 13.00000000000000355 ) ) ;
#8527 = CARTESIAN_POINT ( 'NONE',  ( -13.96533075980324234, 8.621071003556515677, 19.78167371608784819 ) ) ;
#8528 = CARTESIAN_POINT ( 'NONE',  ( 1.837501619626329630, -16.30827793483733501, 3.642857142857143238 ) ) ;
#8529 = CARTESIAN_POINT ( 'NONE',  ( 7.027753727702739539, 7.098671581784288698, 10.74886208192140913 ) ) ;
#8530 = CARTESIAN_POINT ( 'NONE',  ( 13.96533075980324234, -8.621071003556521006, 22.78167371608784464 ) ) ;
#8531 = FACE_OUTER_BOUND ( 'NONE', #2061, .T. ) ;
#8532 = CARTESIAN_POINT ( 'NONE',  ( 7.390897758835871301, -7.458344646081617846, 9.501137918078587319 ) ) ;
#8533 = PLANE ( 'NONE',  #6108 ) ;
#8534 = CARTESIAN_POINT ( 'NONE',  ( -8.621071003556675549, 13.96533075980314642, -1.781673716087850634 ) ) ;
#8535 = AXIS2_PLACEMENT_3D ( 'NONE', #1577, #6158, #4575 ) ;
#8536 = ORIENTED_EDGE ( 'NONE', *, *, #9792, .F. ) ;
#8537 = CARTESIAN_POINT ( 'NONE',  ( 1.737328882695370558, -14.25515036105620581, 5.638816573230711171 ) ) ;
#8538 = CARTESIAN_POINT ( 'NONE',  ( 1.642561882922480621, -10.37072757624892638, 4.800000000000026468 ) ) ;
#8539 = CARTESIAN_POINT ( 'NONE',  ( -1.837501619626328297, 16.30827793483733856, 30.64285714285715301 ) ) ;
#8540 = EDGE_CURVE ( 'NONE', #6270, #7065, #10077, .T. ) ;
#8541 = DIRECTION ( 'NONE',  ( 0.000000000000000000, 0.000000000000000000, 1.000000000000000000 ) ) ;
#8542 = AXIS2_PLACEMENT_3D ( 'NONE', #4602, #10075, #6234 ) ;
#8543 = CARTESIAN_POINT ( 'NONE',  ( -8.877401133907129704, 4.579542530753039742, 10.85113791807856209 ) ) ;
#8544 = CARTESIAN_POINT ( 'NONE',  ( -1.612135949262737844, -9.858066664633888365, 0.9511379180785689558 ) ) ;
#8545 = CARTESIAN_POINT ( 'NONE',  ( -164.3050676404916715, -2.039477515547296171, 12.83914065986469488 ) ) ;
#8546 = CARTESIAN_POINT ( 'NONE',  ( -12.15899005565164792, 7.639999817571651697, 41.78571428571430602 ) ) ;
#8547 = CARTESIAN_POINT ( 'NONE',  ( -14.25515036105622890, 1.737328882695209575, 3.361183426769288385 ) ) ;
#8548 = ORIENTED_EDGE ( 'NONE', *, *, #740, .F. ) ;
#8549 = CARTESIAN_POINT ( 'NONE',  ( 5.404401153735178376, -15.06016580658422477, 11.42453085894499587 ) ) ;
#8550 = DIRECTION ( 'NONE',  ( -1.000000000000000000, -0.000000000000000000, -0.000000000000000000 ) ) ;
#8551 = CARTESIAN_POINT ( 'NONE',  ( -15.49051278174638036, -5.420364854932175902, 34.92857142857145192 ) ) ;
#8552 = CARTESIAN_POINT ( 'NONE',  ( -58.00000000000001421, 0.000000000000000000, 8.200000000000001066 ) ) ;
#8553 = FACE_OUTER_BOUND ( 'NONE', #8059, .T. ) ;
#8554 = CARTESIAN_POINT ( 'NONE',  ( -8.900167166472156666, 4.534861676072231340, 8.850000000000008527 ) ) ;
#8555 = CARTESIAN_POINT ( 'NONE',  ( -1.533232399700100057, 9.375578539472094519, 19.29886208192143471 ) ) ;
#8556 = DIRECTION ( 'NONE',  ( -0.7071067811865510144, 0.7071067811865440200, -6.116266257073745883E-17 ) ) ;
#8557 = CARTESIAN_POINT ( 'NONE',  ( -1.837501619626328297, 16.30827793483733856, 42.64285714285715301 ) ) ;
#8558 = DIRECTION ( 'NONE',  ( -1.000000000000000000, -1.040834085586086106E-16, -6.090254278793936846E-33 ) ) ;
#8559 = CARTESIAN_POINT ( 'NONE',  ( -11.69682198916834892, -11.51250119794901394, 14.50404056962643651 ) ) ;
#8560 = CARTESIAN_POINT ( 'NONE',  ( -15.49051278174638036, -5.420364854932175902, 16.92857142857143771 ) ) ;
#8561 = DIRECTION ( 'NONE',  ( -1.000000000000000000, 0.000000000000000000, 0.000000000000000000 ) ) ;
#8562 = CARTESIAN_POINT ( 'NONE',  ( 4.766900247265192903, 9.355568503977902850, 12.59999999999999964 ) ) ;
#8563 = ORIENTED_EDGE ( 'NONE', *, *, #8294, .T. ) ;
#8564 = CARTESIAN_POINT ( 'NONE',  ( -15.89939535829186923, -1.791431617653016062, 47.14285714285714590 ) ) ;
#8565 = DIRECTION ( 'NONE',  ( 0.000000000000000000, 0.000000000000000000, 1.000000000000000000 ) ) ;
#8566 = EDGE_CURVE ( 'NONE', #5977, #6851, #4964, .T. ) ;
#8567 = CARTESIAN_POINT ( 'NONE',  ( 10.37818827243067510, -1.595456901104500780, 5.198862081921453715 ) ) ;
#8568 = CARTESIAN_POINT ( 'NONE',  ( 13.54758718765249803, 8.512513224245457977, 7.714285714285715301 ) ) ;
#8569 = CARTESIAN_POINT ( 'NONE',  ( -13.82664651025767100, 8.841785722321537477, 45.78975485534073897 ) ) ;
#8570 = CONTEXT_DEPENDENT_SHAPE_REPRESENTATION ( #9639, #5323 ) ;
#8571 = CARTESIAN_POINT ( 'NONE',  ( 1.607813917173037899, -14.26974319298267169, 27.64285714285714590 ) ) ;
#8572 = CARTESIAN_POINT ( 'NONE',  ( -1.486127417882243895, 9.383039235653816590, 12.29999999999997762 ) ) ;
#8573 = ORIENTED_EDGE ( 'NONE', *, *, #6088, .T. ) ;
#8574 = CARTESIAN_POINT ( 'NONE',  ( -9.989344678689363377, 9.809645194533960222, 37.99595943037355994 ) ) ;
#8575 = ORIENTED_EDGE ( 'NONE', *, *, #5911, .T. ) ;
#8576 = DIRECTION ( 'NONE',  ( -0.7056782240951883223, -0.7056782240951970930, -0.06353336191096711771 ) ) ;
#8577 = CARTESIAN_POINT ( 'NONE',  ( -8.404922754268618235, -13.61519076058357491, 24.28167371608785530 ) ) ;
#8578 = CARTESIAN_POINT ( 'NONE',  ( 15.10213328493390783, -5.284464991282587398, 8.571428571428569398 ) ) ;
#8579 = CARTESIAN_POINT ( 'NONE',  ( -9.390499931835536884, 1.439022436064298249, 9.698862081921454603 ) ) ;
#8580 = CARTESIAN_POINT ( 'NONE',  ( -1.967016585148659846, 16.29368510291087091, 26.63881657323070939 ) ) ;
#8581 = CARTESIAN_POINT ( 'NONE',  ( -7.424621202458789426, 7.424621202458720148, 3.000000000000002665 ) ) ;
#8582 = CARTESIAN_POINT ( 'NONE',  ( -9.377220287598998283, -4.724406229267462898, 16.40113791807857524 ) ) ;
#8583 = ADVANCED_FACE ( 'NONE', ( #644 ), #3793, .F. ) ;
#8584 = CYLINDRICAL_SURFACE ( 'NONE', #19, 1.816100000000000270 ) ;
#8585 = AXIS2_PLACEMENT_3D ( 'NONE', #7158, #2404, #76 ) ;
#8586 = ORIENTED_EDGE ( 'NONE', *, *, #7867, .F. ) ;
#8587 = CARTESIAN_POINT ( 'NONE',  ( 4.619798703721856192, 13.59724543428036725, 9.067388001802141773 ) ) ;
#8588 = ORIENTED_EDGE ( 'NONE', *, *, #6836, .F. ) ;
#8589 = CARTESIAN_POINT ( 'NONE',  ( 5.012215536711512875, -9.837026868206002916, 7.649999999999992362 ) ) ;
#8590 = CARTESIAN_POINT ( 'NONE',  ( 13.54758718765249803, 8.512513224245457977, 25.71428571428571885 ) ) ;
#8591 = PLANE ( 'NONE',  #3676 ) ;
#8592 = CARTESIAN_POINT ( 'NONE',  ( 4.967534682030706250, -9.859792900771036983, 9.651137918078598332 ) ) ;
#8594 = AXIS2_PLACEMENT_3D ( 'NONE', #5234, #6767, #6666 ) ;
#8593 = CARTESIAN_POINT ( 'NONE',  ( 8.486213763410640709, 4.270415729527940130, 2.901137918078569466 ) ) ;
#8595 = AXIS2_PLACEMENT_3D ( 'NONE', #9581, #7144, #8068 ) ;
#8596 = LINE ( 'NONE', #6871, #7430 ) ;
#8597 = CARTESIAN_POINT ( 'NONE',  ( 1.917699372585825790, 15.88516839912900203, 46.86118342676930126 ) ) ;
#8598 = CARTESIAN_POINT ( 'NONE',  ( 4.865839792409144771, 13.51115193377589740, 11.07546914105500768 ) ) ;
#8599 = CARTESIAN_POINT ( 'NONE',  ( 14.25515036105622535, -1.737328882695210241, 0.3611834267692887734 ) ) ;
#8600 = ORIENTED_EDGE ( 'NONE', *, *, #8259, .F. ) ;
#8601 = CARTESIAN_POINT ( 'NONE',  ( 11.51250119794888249, 11.69682198916847682, 15.49595943037356882 ) ) ;
#8602 = VECTOR ( 'NONE', #8137, 1000.000000000000000 ) ;
#8603 = DIRECTION ( 'NONE',  ( 1.000000000000000000, 0.000000000000000000, 0.000000000000000000 ) ) ;
#8604 = CIRCLE ( 'NONE', #6756, 15.99999999999999289 ) ;
#8605 = CARTESIAN_POINT ( 'NONE',  ( -1.837501619626328297, 16.30827793483733856, 42.64285714285715301 ) ) ;
#8606 = LINE ( 'NONE', #7153, #5631 ) ;
#8607 = CARTESIAN_POINT ( 'NONE',  ( -88.00000000000002842, 0.000000000000000000, 13.00000000000000000 ) ) ;
#8608 = CARTESIAN_POINT ( 'NONE',  ( 7.098671581784200768, 7.027753727702831021, -0.2488620819214366897 ) ) ;
#8609 = CARTESIAN_POINT ( 'NONE',  ( -4.579542530753125895, 8.877401133907083519, 13.14886208192146633 ) ) ;
#8610 = ADVANCED_FACE ( 'NONE', ( #3059, #6203 ), #8902, .T. ) ;
#8611 = DIRECTION ( 'NONE',  ( 0.000000000000000000, -6.338944243255235518E-49, 1.000000000000000000 ) ) ;
#8612 = CARTESIAN_POINT ( 'NONE',  ( 8.621071003556677326, -13.96533075980314287, 19.21832628391215181 ) ) ;
#8613 = CARTESIAN_POINT ( 'NONE',  ( 4.995402070941135086, -13.58603705635637304, -1.270000000000007123 ) ) ;
#8614 = MECHANICAL_DESIGN_GEOMETRIC_PRESENTATION_REPRESENTATION (  '', ( #7792 ), #358 ) ;
#8615 = CARTESIAN_POINT ( 'NONE',  ( -1.917699372585823570, -15.88516839912900558, 13.86118342676929416 ) ) ;
#8616 = CARTESIAN_POINT ( 'NONE',  ( -5.284464991282755264, 15.10213328493384743, 12.42857142857142705 ) ) ;
#8617 = CARTESIAN_POINT ( 'NONE',  ( -170.0000000000000284, -1.448262861947153525E-15, 0.000000000000000000 ) ) ;
#8618 = ORIENTED_EDGE ( 'NONE', *, *, #9912, .F. ) ;
#8619 = CARTESIAN_POINT ( 'NONE',  ( 11.31370849898482334, -11.31370849898469366, 3.000000000000002665 ) ) ;
#8620 = AXIS2_PLACEMENT_3D ( 'NONE', #5249, #10013, #4541 ) ;
#8621 = CARTESIAN_POINT ( 'NONE',  ( -11.60466159355861748, -11.60466159355874893, 46.50000000000001421 ) ) ;
#8622 = AXIS2_PLACEMENT_3D ( 'NONE', #8790, #7178, #95 ) ;
#8623 = FILL_AREA_STYLE_COLOUR ( '', #8207 ) ;
#8624 = CARTESIAN_POINT ( 'NONE',  ( 10.37818827243067510, -1.595456901104500780, 8.198862081921454603 ) ) ;
#8625 = CARTESIAN_POINT ( 'NONE',  ( -15.89939535829186923, -1.791431617653016062, 5.142857142857143238 ) ) ;
#8626 = CARTESIAN_POINT ( 'NONE',  ( 13.89598863503046111, -8.731428362939032795, 2.785714285714284255 ) ) ;
#8627 = CONTEXT_DEPENDENT_SHAPE_REPRESENTATION ( #9829, #9948 ) ;
#8628 = CARTESIAN_POINT ( 'NONE',  ( 9.899494936611718643, -9.899494936611608509, 45.00000000000000711 ) ) ;
#8629 = CARTESIAN_POINT ( 'NONE',  ( 1.562606840307832146, 9.865911304835508489, 12.44999999999995666 ) ) ;
#8630 = CARTESIAN_POINT ( 'NONE',  ( 1.642561882922480621, -10.37072757624892638, 16.80000000000003624 ) ) ;
#8631 = ORIENTED_EDGE ( 'NONE', *, *, #8210, .T. ) ;
#8632 = CARTESIAN_POINT ( 'NONE',  ( 13.91197093850538380, 1.567502665446386390, 8.142857142857145902 ) ) ;
#8633 = ORIENTED_EDGE ( 'NONE', *, *, #9584, .T. ) ;
#8634 = PLANE ( 'NONE',  #5727 ) ;
#8635 = CARTESIAN_POINT ( 'NONE',  ( -16.32287076676382398, 1.707986654103809343, 19.35310228751642825 ) ) ;
#8636 = LINE ( 'NONE', #7756, #5494 ) ;
#8637 = CIRCLE ( 'NONE', #4174, 1.535500000000000087 ) ;
#8638 = CARTESIAN_POINT ( 'NONE',  ( 11.51250119794888249, 11.69682198916847682, 21.49595943037356705 ) ) ;
#8639 = FACE_OUTER_BOUND ( 'NONE', #9147, .T. ) ;
#8640 = CARTESIAN_POINT ( 'NONE',  ( 1.642561882922480621, -10.37072757624892638, 1.800000000000023803 ) ) ;
#8641 = EDGE_CURVE ( 'NONE', #8413, #6851, #3218, .T. ) ;
#8642 = CARTESIAN_POINT ( 'NONE',  ( 12.15899005565164792, -7.639999817571654361, 2.785714285714283367 ) ) ;
#8643 = VERTEX_POINT ( 'NONE', #62 ) ;
#8644 = CARTESIAN_POINT ( 'NONE',  ( -11.51250119794888072, -11.69682198916848037, 48.49595943037355994 ) ) ;
#8645 = CARTESIAN_POINT ( 'NONE',  ( -10.37072757624895836, 1.642561882922380923, 2.699999999999980194 ) ) ;
#8646 = FACE_OUTER_BOUND ( 'NONE', #571, .T. ) ;
#8647 = CARTESIAN_POINT ( 'NONE',  ( 1.737328882695370558, -14.25515036105620581, 23.63881657323070939 ) ) ;
#8648 = CARTESIAN_POINT ( 'NONE',  ( -10.91227292449344155, -1.677562661911747632, 1.551137918078593803 ) ) ;
#8649 = CARTESIAN_POINT ( 'NONE',  ( 9.375578539472099848, -1.533232399699986370, 18.20113791807854398 ) ) ;
#8650 = CARTESIAN_POINT ( 'NONE',  ( -162.9065109726407456, -0.5641505380384801427, 12.99034143968891541 ) ) ;
#8651 = CARTESIAN_POINT ( 'NONE',  ( -1.478298951650703019, 14.28433602490913579, 10.64689771248357886 ) ) ;
#8652 = PRODUCT_DEFINITION ( 'UNKNOWN', '', #4103, #4021 ) ;
#8653 = CARTESIAN_POINT ( 'NONE',  ( -7.529642458189277576, 12.22833218042435455, 16.21832628391214470 ) ) ;
#8654 = ORIENTED_EDGE ( 'NONE', *, *, #2119, .F. ) ;
#8655 = CARTESIAN_POINT ( 'NONE',  ( 15.88516839912898071, 1.917699372586004092, 10.13881657323070762 ) ) ;
#8656 = DIRECTION ( 'NONE',  ( -1.000000000000000000, -1.387778780781445676E-16, -0.000000000000000000 ) ) ;
#8657 = CARTESIAN_POINT ( 'NONE',  ( -15.49051278174638036, -5.420364854932175902, 46.92857142857142350 ) ) ;
#8658 = VECTOR ( 'NONE', #3788, 1000.000000000000000 ) ;
#8659 = CARTESIAN_POINT ( 'NONE',  ( -160.0000000000000284, -15.00000000000000711, 1.836970198721029589E-15 ) ) ;
#8660 = CARTESIAN_POINT ( 'NONE',  ( -1.612135949262737844, -9.858066664633888365, 0.9511379180785689558 ) ) ;
#8661 = CARTESIAN_POINT ( 'NONE',  ( -9.390499931835536884, 1.439022436064298249, 18.69886208192145816 ) ) ;
#8662 = DIRECTION ( 'NONE',  ( 1.000000000000000000, 4.755747939841215952E-17, -0.000000000000000000 ) ) ;
#8663 = CARTESIAN_POINT ( 'NONE',  ( -11.69682198916834892, -11.51250119794901394, 32.50404056962644006 ) ) ;
#8664 = CARTESIAN_POINT ( 'NONE',  ( -68.00000000000002842, 0.000000000000000000, 18.00000000000000355 ) ) ;
#8665 = CARTESIAN_POINT ( 'NONE',  ( -13.61519076058348254, -8.404922754268771001, 32.71832628391215536 ) ) ;
#8666 = CARTESIAN_POINT ( 'NONE',  ( -11.60466159355861926, -11.60466159355875249, 16.50000000000000000 ) ) ;
#8667 = CARTESIAN_POINT ( 'NONE',  ( 61.99999999999997158, 0.000000000000000000, 0.000000000000000000 ) ) ;
#8668 = CYLINDRICAL_SURFACE ( 'NONE', #675, 16.99999999999997868 ) ;
#8669 = EDGE_CURVE ( 'NONE', #3042, #4989, #5640, .T. ) ;
#8670 =( NAMED_UNIT ( * ) PLANE_ANGLE_UNIT ( ) SI_UNIT ( $, .RADIAN. ) );
#8671 = DIRECTION ( 'NONE',  ( 1.000000000000000000, 0.000000000000000000, 0.000000000000000000 ) ) ;
#8672 = ADVANCED_FACE ( 'NONE', ( #844 ), #3999, .T. ) ;
#8673 = UNCERTAINTY_MEASURE_WITH_UNIT (LENGTH_MEASURE( 1.000000000000000082E-05 ), #1544, 'distance_accuracy_value', 'NONE');
#8674 = CARTESIAN_POINT ( 'NONE',  ( -4.724406229267374968, -9.377220287599040915, 6.098862081921437195 ) ) ;
#8675 = CARTESIAN_POINT ( 'NONE',  ( -7.556039541191334585, -11.78653521626503320, 44.28975485534073186 ) ) ;
#8676 = CARTESIAN_POINT ( 'NONE',  ( 5.420364854932001819, 15.49051278174644430, 13.07142857142857295 ) ) ;
#8677 = CARTESIAN_POINT ( 'NONE',  ( 12.15899005565164792, -7.639999817571654361, 38.78571428571429180 ) ) ;
#8678 = CARTESIAN_POINT ( 'NONE',  ( -4.312909747525649706, -8.464561979789507973, 14.10000000000000142 ) ) ;
#8679 = CARTESIAN_POINT ( 'NONE',  ( 10.37818827243067510, -1.595456901104499448, 2.198862081921450606 ) ) ;
#8680 = ORIENTED_EDGE ( 'NONE', *, *, #8067, .F. ) ;
#8681 = CARTESIAN_POINT ( 'NONE',  ( 1.607813917173038121, -14.26974319298267346, 9.642857142857147679 ) ) ;
#8682 = DIRECTION ( 'NONE',  ( -1.000000000000000000, -0.000000000000000000, -0.000000000000000000 ) ) ;
#8683 = CARTESIAN_POINT ( 'NONE',  ( -13.47998361472151174, -8.620103694222146729, 30.71024514465928235 ) ) ;
#8684 = CARTESIAN_POINT ( 'NONE',  ( 13.54758718765249803, 8.512513224245457977, 19.71428571428571175 ) ) ;
#8685 = CARTESIAN_POINT ( 'NONE',  ( -5.404401153735176599, 15.06016580658422477, 26.42453085894499765 ) ) ;
#8686 = CARTESIAN_POINT ( 'NONE',  ( 7.424621202458790314, -7.424621202458697944, 1.500000000000001332 ) ) ;
#8687 = CARTESIAN_POINT ( 'NONE',  ( -10.37072757624895836, 1.642561882922380923, 2.699999999999980194 ) ) ;
#8688 = FACE_OUTER_BOUND ( 'NONE', #3138, .T. ) ;
#8689 = SURFACE_SIDE_STYLE ('',( #4810 ) ) ;
#8690 = EDGE_LOOP ( 'NONE', ( #2063, #4040 ) ) ;
#8691 = CARTESIAN_POINT ( 'NONE',  ( -11.78653521626494793, -7.556039541191465148, 18.71024514465927879 ) ) ;
#8692 = EDGE_CURVE ( 'NONE', #285, #4852, #8756, .T. ) ;
#8693 = CARTESIAN_POINT ( 'NONE',  ( -9.355568503977838901, -4.766900247265279944, 11.39999999999996660 ) ) ;
#8694 = CYLINDRICAL_SURFACE ( 'NONE', #3210, 13.00000000000000000 ) ;
#8695 = CARTESIAN_POINT ( 'NONE',  ( 13.51115193377584589, 4.865839792409294873, 27.92453085894499054 ) ) ;
#8696 = CARTESIAN_POINT ( 'NONE',  ( -10.36326688006724162, 1.689666864740236640, 1.701137918078535094 ) ) ;
#8697 = CARTESIAN_POINT ( 'NONE',  ( 6.683790977649321619, -6.751237864895076157, 15.50113791807859620 ) ) ;
#8698 = EDGE_CURVE ( 'NONE', #8824, #6875, #5539, .T. ) ;
#8699 = CARTESIAN_POINT ( 'NONE',  ( -2.000000000000001776, 20.00000000000000000, 0.000000000000000000 ) ) ;
#8700 = CARTESIAN_POINT ( 'NONE',  ( 10.24623928997352884, 10.06191849875416899, 11.50404056962644006 ) ) ;
#8701 = CARTESIAN_POINT ( 'NONE',  ( 7.529642458189280241, -12.22833218042435099, 19.21832628391215181 ) ) ;
#8702 = ORIENTED_EDGE ( 'NONE', *, *, #3738, .T. ) ;
#8703 = LINE ( 'NONE', #649, #6687 ) ;
#8704 = CARTESIAN_POINT ( 'NONE',  ( 8.512513224245308763, 13.54758718765259040, 49.28571428571428470 ) ) ;
#8705 = CARTESIAN_POINT ( 'NONE',  ( 0.000000000000000000, 0.000000000000000000, -1.270000000000007123 ) ) ;
#8706 = FACE_OUTER_BOUND ( 'NONE', #5999, .T. ) ;
#8707 = CARTESIAN_POINT ( 'NONE',  ( 9.383039235653818366, -1.486127417882131097, 16.19999999999999218 ) ) ;
#8708 = CARTESIAN_POINT ( 'NONE',  ( 4.534861676072320158, -8.900167166472096270, 7.649999999999992362 ) ) ;
#8709 = CARTESIAN_POINT ( 'NONE',  ( -163.9213440228380989, 1.865096155104054354, 12.86575230306539908 ) ) ;
#8710 = CARTESIAN_POINT ( 'NONE',  ( 15.06016580658428694, -5.404401153735007846, 24.57546914105500946 ) ) ;
#8711 = DIRECTION ( 'NONE',  ( 1.000000000000000000, 4.755747939841215952E-17, -0.000000000000000000 ) ) ;
#8712 = CARTESIAN_POINT ( 'NONE',  ( -1.707986654103994528, 16.32287076676380266, 34.64689771248358596 ) ) ;
#8713 = VERTEX_POINT ( 'NONE', #7914 ) ;
#8714 = CARTESIAN_POINT ( 'NONE',  ( 15.10213328493390783, -5.284464991282587398, 26.57142857142857295 ) ) ;
#8715 = CARTESIAN_POINT ( 'NONE',  ( 0.7290266316634184118, 15.99096059591463614, 48.73000000000001108 ) ) ;
#8716 = CARTESIAN_POINT ( 'NONE',  ( 15.89939535829187278, 1.791431617653015174, 2.142857142857140573 ) ) ;
#8717 = CARTESIAN_POINT ( 'NONE',  ( 0.000000000000000000, -0.8865213383406761460, 1.535499999999911935 ) ) ;
#8718 = SURFACE_STYLE_FILL_AREA ( #5558 ) ;
#8719 = CARTESIAN_POINT ( 'NONE',  ( 4.579542530753127672, -8.877401133907065756, 2.648862081921448119 ) ) ;
#8720 = AXIS2_PLACEMENT_3D ( 'NONE', #4543, #7697, #7269 ) ;
#8721 = CARTESIAN_POINT ( 'NONE',  ( -4.724406229267374968, -9.377220287599046245, 12.09886208192144252 ) ) ;
#8722 = CARTESIAN_POINT ( 'NONE',  ( 7.529642458189280241, -12.22833218042435099, 43.21832628391217668 ) ) ;
#8723 = CARTESIAN_POINT ( 'NONE',  ( -8.512513224245306986, -13.54758718765259218, 10.28571428571428648 ) ) ;
#8724 = CONTEXT_DEPENDENT_SHAPE_REPRESENTATION ( #5723, #3577 ) ;
#8725 = CARTESIAN_POINT ( 'NONE',  ( -13.55419868402807992, -4.742819248065651472, 40.92857142857143771 ) ) ;
#8726 = CARTESIAN_POINT ( 'NONE',  ( 13.17239914596754424, -4.743843029824685864, 42.57546914105501656 ) ) ;
#8727 = CARTESIAN_POINT ( 'NONE',  ( -11.92174236212692051, -7.340858601238089420, 32.71832628391215536 ) ) ;
#8728 = CARTESIAN_POINT ( 'NONE',  ( -1.486127417882243895, 9.383039235653825472, 9.299999999999975842 ) ) ;
#8729 = CARTESIAN_POINT ( 'NONE',  ( -7.424621202458789426, 7.424621202458723701, 15.00000000000001421 ) ) ;
#8730 = ORIENTED_EDGE ( 'NONE', *, *, #2171, .F. ) ;
#8731 = CARTESIAN_POINT ( 'NONE',  ( 9.899494936611718643, -9.899494936611608509, 3.000000000000002665 ) ) ;
#8732 = VERTEX_POINT ( 'NONE', #4819 ) ;
#8733 = DIRECTION ( 'NONE',  ( 1.000000000000000000, 0.000000000000000000, 0.000000000000000000 ) ) ;
#8734 = CARTESIAN_POINT ( 'NONE',  ( 11.31370849898482334, -11.31370849898469366, 21.00000000000000355 ) ) ;
#8735 = CARTESIAN_POINT ( 'NONE',  ( -11.40355824106246807, 11.22385875690704715, 25.99595943037356349 ) ) ;
#8736 = CARTESIAN_POINT ( 'NONE',  ( -10.37072757624895836, 1.642561882922380923, 2.699999999999980194 ) ) ;
#8737 = CARTESIAN_POINT ( 'NONE',  ( 1.727091770866550968, 10.90442828429187294, 3.450000000000006839 ) ) ;
#8738 = CARTESIAN_POINT ( 'NONE',  ( -4.623906867372410190, 13.21436662431711895, 0.4285714285714309346 ) ) ;
#8739 = SHAPE_REPRESENTATION_RELATIONSHIP ( 'NONE' , 'NONE' ,  #1843, #9458 ) ;
#8740 = EDGE_LOOP ( 'NONE', ( #233, #29, #3663, #7186, #3596 ) ) ;
#8741 = CARTESIAN_POINT ( 'NONE',  ( 12.22833218042443271, -7.529642458189144349, 10.78167371608784819 ) ) ;
#8742 = CARTESIAN_POINT ( 'NONE',  ( 5.012215536711512875, -9.837026868206002916, 16.64999999999999858 ) ) ;
#8743 = CARTESIAN_POINT ( 'NONE',  ( 8.731428362939190890, -13.89598863503036164, 15.21428571428571530 ) ) ;
#8744 = DIRECTION ( 'NONE',  ( -4.755747939841215952E-17, 1.000000000000000000, 0.000000000000000000 ) ) ;
#8745 = CARTESIAN_POINT ( 'NONE',  ( -1.595456901104623348, 10.37818827243066622, 2.301137918078551614 ) ) ;
#8746 = CARTESIAN_POINT ( 'NONE',  ( 7.098671581784200768, 7.027753727702823916, 14.75113791807856956 ) ) ;
#8747 = CARTESIAN_POINT ( 'NONE',  ( -55.00000000000002132, 9.020562075080166030E-17, 13.00000000000001066 ) ) ;
#8748 = CARTESIAN_POINT ( 'NONE',  ( 14.25515036105622535, -1.737328882695210241, 6.361183426769297711 ) ) ;
#8749 = MECHANICAL_DESIGN_GEOMETRIC_PRESENTATION_REPRESENTATION (  '', ( #6274 ), #4284 ) ;
#8750 = CARTESIAN_POINT ( 'NONE',  ( -11.92174236212692051, -7.340858601238089420, 14.71832628391215003 ) ) ;
#8751 = ORIENTED_EDGE ( 'NONE', *, *, #161, .T. ) ;
#8752 = DIRECTION ( 'NONE',  ( 1.000000000000000000, -4.575525868300071581E-16, -0.000000000000000000 ) ) ;
#8753 = CARTESIAN_POINT ( 'NONE',  ( -11.60466159355861926, -11.60466159355875249, 40.50000000000000711 ) ) ;
#8754 = CARTESIAN_POINT ( 'NONE',  ( 2.886521338340691578, 0.000000000000000000, 0.000000000000000000 ) ) ;
#8755 = CARTESIAN_POINT ( 'NONE',  ( 14.00000000000000533, 0.000000000000000000, 0.000000000000000000 ) ) ;
#8756 = CIRCLE ( 'NONE', #7268, 0.9906000000000003691 ) ;
#8757 = CARTESIAN_POINT ( 'NONE',  ( 4.355403765523470305, 8.442910196168369907, -0.3988620819214416247 ) ) ;
#8758 = CARTESIAN_POINT ( 'NONE',  ( 7.063212654743467489, 7.063212654743557195, 6.749999999999960032 ) ) ;
#8759 = CARTESIAN_POINT ( 'NONE',  ( -167.1500000000000341, 0.1423186749851698130, 13.00000000000000000 ) ) ;
#8760 = CARTESIAN_POINT ( 'NONE',  ( 16.29368510291089223, -1.967016585148476882, 24.36118342676929416 ) ) ;
#8761 = CARTESIAN_POINT ( 'NONE',  ( 7.063212654743468377, 7.063212654743559860, 3.749999999999997780 ) ) ;
#8762 = CARTESIAN_POINT ( 'NONE',  ( 13.61519076058348254, 8.404922754268771001, 29.71832628391214826 ) ) ;
#8763 = VECTOR ( 'NONE', #3431, 1000.000000000000000 ) ;
#8764 = AXIS2_PLACEMENT_3D ( 'NONE', #6114, #758, #5503 ) ;
#8765 = CIRCLE ( 'NONE', #8108, 16.00000000000000000 ) ;
#8766 = ORIENTED_EDGE ( 'NONE', *, *, #6657, .F. ) ;
#8767 = CARTESIAN_POINT ( 'NONE',  ( 1.791431617652837316, 15.89939535829188877, 36.85714285714286120 ) ) ;
#8768 = CARTESIAN_POINT ( 'NONE',  ( 3.924309341735328527, 14.50897616450780170, 2.434022981070398477E-13 ) ) ;
#8769 = CARTESIAN_POINT ( 'NONE',  ( 0.000000000000000000, 0.000000000000000000, 0.000000000000000000 ) ) ;
#8770 = APPLICATION_CONTEXT ( 'automotive_design' ) ;
#8771 = FILL_AREA_STYLE ('',( #7990 ) ) ;
#8772 =( LENGTH_UNIT ( ) NAMED_UNIT ( * ) SI_UNIT ( .MILLI., .METRE. ) );
#8773 = AXIS2_PLACEMENT_3D ( 'NONE', #1527, #2198, #6309 ) ;
#8774 = CARTESIAN_POINT ( 'NONE',  ( -9.858066664633883036, -1.612135949262831547, 6.548862081921412504 ) ) ;
#8775 = CARTESIAN_POINT ( 'NONE',  ( 7.458344646081711105, -7.390897758835778930, 14.49886208192142867 ) ) ;
#8776 = CIRCLE ( 'NONE', #1341, 20.00000000000000000 ) ;
#8777 = MECHANICAL_DESIGN_GEOMETRIC_PRESENTATION_REPRESENTATION (  '', ( #7446 ), #192 ) ;
#8778 = UNCERTAINTY_MEASURE_WITH_UNIT (LENGTH_MEASURE( 1.000000000000000082E-05 ), #6881, 'distance_accuracy_value', 'NONE');
#8779 = CARTESIAN_POINT ( 'NONE',  ( -4.724406229267374968, -9.377220287599040915, 15.09886208192144430 ) ) ;
#8780 = CARTESIAN_POINT ( 'NONE',  ( -11.69682198916834892, -11.51250119794901394, 2.504040569626438728 ) ) ;
#8781 = CARTESIAN_POINT ( 'NONE',  ( -15.89939535829186923, -1.791431617653016062, 11.14285714285714235 ) ) ;
#8782 = CARTESIAN_POINT ( 'NONE',  ( 1.567502665446232957, 13.91197093850540156, 42.85714285714285410 ) ) ;
#8783 = CARTESIAN_POINT ( 'NONE',  ( -14.25515036105622890, 1.737328882695209575, 39.36118342676930837 ) ) ;
#8784 = CARTESIAN_POINT ( 'NONE',  ( 7.639999817571789364, -12.15899005565156266, 9.214285714285717077 ) ) ;
#8785 = CARTESIAN_POINT ( 'NONE',  ( -6.717514421272238856, 6.717514421272181124, 18.00000000000001421 ) ) ;
#8786 =( GEOMETRIC_REPRESENTATION_CONTEXT ( 3 ) GLOBAL_UNCERTAINTY_ASSIGNED_CONTEXT ( ( #193 ) ) GLOBAL_UNIT_ASSIGNED_CONTEXT ( ( #7498, #3675, #3464 ) ) REPRESENTATION_CONTEXT ( 'NONE', 'WORKASPACE' ) );
#8787 = CARTESIAN_POINT ( 'NONE',  ( 9.355568503977840678, 4.766900247265305701, 12.90000000000002345 ) ) ;
#8788 = ORIENTED_EDGE ( 'NONE', *, *, #5893, .T. ) ;
#8789 = CARTESIAN_POINT ( 'NONE',  ( -1.607813917173034124, 14.26974319298267524, 6.642857142857143238 ) ) ;
#8790 = CARTESIAN_POINT ( 'NONE',  ( -68.00000000000002842, 0.000000000000000000, 0.000000000000000000 ) ) ;
#8791 = CARTESIAN_POINT ( 'NONE',  ( -13.89598863503045933, 8.731428362939027465, 17.78571428571428825 ) ) ;
#8792 = CARTESIAN_POINT ( 'NONE',  ( 13.96533075980324234, -8.621071003556521006, 40.78167371608785885 ) ) ;
#8793 = CARTESIAN_POINT ( 'NONE',  ( -7.424621202458789426, 7.424621202458724589, 12.00000000000001066 ) ) ;
#8794 = CARTESIAN_POINT ( 'NONE',  ( 7.424621202458790314, -7.424621202458697944, 1.500000000000001332 ) ) ;
#8795 = CARTESIAN_POINT ( 'NONE',  ( 56.99999999999997158, 8.572527594031471218E-16, -6.999999999999999112 ) ) ;
#8796 = TOROIDAL_SURFACE ( 'NONE', #1526, 8.000000000000000000, 1.000000000000000888 ) ;
#8797 = DIRECTION ( 'NONE',  ( 1.000000000000000000, 0.000000000000000000, 0.000000000000000000 ) ) ;
#8798 = VERTEX_POINT ( 'NONE', #8747 ) ;
#8799 = CARTESIAN_POINT ( 'NONE',  ( 10.06191849875406064, 10.24623928997363187, 15.49595943037356882 ) ) ;
#8800 = CARTESIAN_POINT ( 'NONE',  ( 7.424621202458790314, -7.424621202458697944, 16.50000000000001421 ) ) ;
#8801 = EDGE_CURVE ( 'NONE', #3628, #4031, #7604, .T. ) ;
#8802 = CARTESIAN_POINT ( 'NONE',  ( -163.3607213683654606, 0.2164297246728172364, 12.99862687051388832 ) ) ;
#8803 = CARTESIAN_POINT ( 'NONE',  ( -1.837501619626328297, 16.30827793483733856, 36.64285714285714590 ) ) ;
#8804 = CARTESIAN_POINT ( 'NONE',  ( 4.619798703721856192, 13.59724543428036725, 45.06738800180215065 ) ) ;
#8805 = CARTESIAN_POINT ( 'NONE',  ( -10.91227292449344155, -1.677562661911748965, 7.551137918078578259 ) ) ;
#8806 = CARTESIAN_POINT ( 'NONE',  ( -1.439022436064386845, 9.390499931835535108, 14.30113791807856316 ) ) ;
#8807 = EDGE_CURVE ( 'NONE', #1810, #4112, #3146, .T. ) ;
#8808 = CARTESIAN_POINT ( 'NONE',  ( -158.0000000000000284, 17.99999999999999645, 0.000000000000000000 ) ) ;
#8809 = CARTESIAN_POINT ( 'NONE',  ( 13.59724543428031573, 4.619798703722006294, 5.932611998197868886 ) ) ;
#8810 =( NAMED_UNIT ( * ) PLANE_ANGLE_UNIT ( ) SI_UNIT ( $, .RADIAN. ) );
#8811 = AXIS2_PLACEMENT_3D ( 'NONE', #276, #954, #7353 ) ;
#8812 = CARTESIAN_POINT ( 'NONE',  ( 14.25515036105622535, -1.737328882695210241, 6.361183426769297711 ) ) ;
#8813 = ORIENTED_EDGE ( 'NONE', *, *, #3, .F. ) ;
#8814 = DIRECTION ( 'NONE',  ( -1.000000000000000000, 0.000000000000000000, 0.000000000000000000 ) ) ;
#8815 = CARTESIAN_POINT ( 'NONE',  ( 5.404401153735178376, -15.06016580658422477, 11.42453085894499587 ) ) ;
#8816 = DIRECTION ( 'NONE',  ( -1.000000000000000000, -0.000000000000000000, -0.000000000000000000 ) ) ;
#8817 = DIRECTION ( 'NONE',  ( 1.000000000000000000, 4.755747939841215952E-17, -0.000000000000000000 ) ) ;
#8818 = CARTESIAN_POINT ( 'NONE',  ( 7.063212654743467489, 7.063212654743553642, 15.74999999999996803 ) ) ;
#8819 = CARTESIAN_POINT ( 'NONE',  ( 6.717514421272239744, -6.717514421272154479, 10.50000000000000888 ) ) ;
#8820 = CARTESIAN_POINT ( 'NONE',  ( -167.0397669596979426, 0.6940490614466876540, 12.98211462413728157 ) ) ;
#8821 = CARTESIAN_POINT ( 'NONE',  ( -15.91362231745475597, -1.665163862720028254, 27.14689771248358241 ) ) ;
#8822 = DIRECTION ( 'NONE',  ( -1.000000000000000000, -0.000000000000000000, -0.000000000000000000 ) ) ;
#8823 = CARTESIAN_POINT ( 'NONE',  ( -15.06016580658428694, 5.404401153735006957, 27.57546914105500946 ) ) ;
#8824 = VERTEX_POINT ( 'NONE', #8808 ) ;
#8825 = CARTESIAN_POINT ( 'NONE',  ( 15.49051278174638036, 5.420364854932175014, 31.92857142857143415 ) ) ;
#8826 = CARTESIAN_POINT ( 'NONE',  ( 3.654384819347590962, 14.75870095501612944, 2.020632658447807793E-13 ) ) ;
#8827 = CARTESIAN_POINT ( 'NONE',  ( 1.791431617652837316, 15.89939535829188877, 6.857142857142860315 ) ) ;
#8828 = EDGE_CURVE ( 'NONE', #8643, #9194, #2805, .T. ) ;
#8829 = CARTESIAN_POINT ( 'NONE',  ( 10.19143222367002366, 10.12210786732603474, 48.73000000000001819 ) ) ;
#8830 = CARTESIAN_POINT ( 'NONE',  ( -8.442910196168309511, -4.355403765523546689, 9.398862081921404155 ) ) ;
#8831 = CARTESIAN_POINT ( 'NONE',  ( 10.37818827243067510, -1.595456901104500780, 17.19886208192146171 ) ) ;
#8832 = CARTESIAN_POINT ( 'NONE',  ( -7.529642458189277576, 12.22833218042435455, 46.21832628391216247 ) ) ;
#8833 = CARTESIAN_POINT ( 'NONE',  ( 13.89598863503046111, -8.731428362939032795, 14.78571428571429358 ) ) ;
#8834 = CARTESIAN_POINT ( 'NONE',  ( -7.639999817571786700, 12.15899005565156266, 42.21428571428571530 ) ) ;
#8835 = CARTESIAN_POINT ( 'NONE',  ( 14.25515036105622535, -1.737328882695210241, 42.36118342676930126 ) ) ;
#8836 = CARTESIAN_POINT ( 'NONE',  ( 14.26974319298268767, -1.607813917172876916, 14.35714285714285587 ) ) ;
#8837 = DIRECTION ( 'NONE',  ( -4.575525868300071581E-16, -1.000000000000000000, 0.000000000000000000 ) ) ;
#8838 = CARTESIAN_POINT ( 'NONE',  ( -9.333916720356675967, -4.809394265263096990, 6.398862081921446787 ) ) ;
#8839 = ORIENTED_EDGE ( 'NONE', *, *, #5600, .T. ) ;
#8840 = CARTESIAN_POINT ( 'NONE',  ( 4.742819248065503146, 13.55419868402813677, 1.071428571428570287 ) ) ;
#8841 = EDGE_LOOP ( 'NONE', ( #1472, #5207 ) ) ;
#8842 = EDGE_CURVE ( 'NONE', #7778, #9360, #7086, .T. ) ;
#8843 = DIRECTION ( 'NONE',  ( 1.000000000000000000, 0.000000000000000000, 0.000000000000000000 ) ) ;
#8844 = CARTESIAN_POINT ( 'NONE',  ( -13.54758718765249625, -8.512513224245459753, 16.71428571428571530 ) ) ;
#8845 = EDGE_CURVE ( 'NONE', #6711, #2258, #10, .T. ) ;
#8846 = CARTESIAN_POINT ( 'NONE',  ( -16.32287076676382398, 1.707986654103809343, 37.35310228751641404 ) ) ;
#8847 = CARTESIAN_POINT ( 'NONE',  ( 10.37072757624895836, -1.642561882922355609, 4.199999999999981526 ) ) ;
#8848 = CARTESIAN_POINT ( 'NONE',  ( -5.012215536711506658, 9.837026868206027785, 3.149999999999957723 ) ) ;
#8849 = CARTESIAN_POINT ( 'NONE',  ( 7.448449071214646722, 11.85413878919601594, 1.285714285714285809 ) ) ;
#8850 = EDGE_LOOP ( 'NONE', ( #4966, #7974 ) ) ;
#8851 = CARTESIAN_POINT ( 'NONE',  ( 13.25633410266679313, -4.503970704919842305, 10.56738800180213644 ) ) ;
#8852 = CARTESIAN_POINT ( 'NONE',  ( -1.642561882922479732, 10.37072757624895303, 12.29999999999997762 ) ) ;
#8853 = FACE_OUTER_BOUND ( 'NONE', #1635, .T. ) ;
#8854 = CARTESIAN_POINT ( 'NONE',  ( 1.737328882695370558, -14.25515036105620581, 35.63881657323071295 ) ) ;
#8855 = CARTESIAN_POINT ( 'NONE',  ( 1.595456901104624459, -10.37818827243064490, 15.80113791807855961 ) ) ;
#8856 = CARTESIAN_POINT ( 'NONE',  ( -1.439022436064386845, 9.390499931835535108, 17.30113791807856316 ) ) ;
#8857 = CARTESIAN_POINT ( 'NONE',  ( -8.560346291714190440E-16, 18.00000000000000355, 0.000000000000000000 ) ) ;
#8858 = CARTESIAN_POINT ( 'NONE',  ( 4.865839792409144771, 13.51115193377589740, 23.07546914105501301 ) ) ;
#8859 = EDGE_LOOP ( 'NONE', ( #5673, #9986, #6103, #9500 ) ) ;
#8860 = DIRECTION ( 'NONE',  ( 0.000000000000000000, -6.338944243255235518E-49, 1.000000000000000000 ) ) ;
#8861 = CARTESIAN_POINT ( 'NONE',  ( -15.88516839912898071, -1.917699372586004980, 13.13881657323070584 ) ) ;
#8862 = CARTESIAN_POINT ( 'NONE',  ( -166.0915134144852345, -1.242040127916074654, 12.94075629995628063 ) ) ;
#8863 = CARTESIAN_POINT ( 'NONE',  ( -58.00000000000002842, 9.473114452887993551E-16, -8.200000000000009948 ) ) ;
#8864 = CARTESIAN_POINT ( 'NONE',  ( 4.355403765523470305, 8.442910196168369907, 8.601137918078563871 ) ) ;
#8865 = CARTESIAN_POINT ( 'NONE',  ( -7.063212654743466601, -7.063212654743534991, 8.250000000000028422 ) ) ;
#8866 = DIRECTION ( 'NONE',  ( 1.000000000000000000, 4.755747939841215952E-17, -0.000000000000000000 ) ) ;
#8867 = CARTESIAN_POINT ( 'NONE',  ( 9.899494936611718643, -9.899494936611608509, 33.00000000000000000 ) ) ;
#8868 = CARTESIAN_POINT ( 'NONE',  ( -11.69682198916834892, -11.51250119794901394, 32.50404056962644006 ) ) ;
#8869 = CIRCLE ( 'NONE', #8200, 8.000000000000000000 ) ;
#8870 = ORIENTED_EDGE ( 'NONE', *, *, #8505, .F. ) ;
#8871 = CARTESIAN_POINT ( 'NONE',  ( 1.837501619626330074, -16.30827793483733501, 33.64285714285715301 ) ) ;
#8872 = CARTESIAN_POINT ( 'NONE',  ( 5.986002070941135678, -13.58603705635637304, 0.000000000000000000 ) ) ;
#8873 = CARTESIAN_POINT ( 'NONE',  ( -15.10213328493390961, 5.284464991282586510, 17.57142857142856940 ) ) ;
#8874 = DIRECTION ( 'NONE',  ( 1.000000000000000000, 0.000000000000000000, 0.000000000000000000 ) ) ;
#8875 = CARTESIAN_POINT ( 'NONE',  ( 8.442910196168311288, 4.355403765523574222, 13.89886208192141126 ) ) ;
#8876 = CARTESIAN_POINT ( 'NONE',  ( 13.89598863503046111, -8.731428362939032795, 38.78571428571429180 ) ) ;
#8877 = CARTESIAN_POINT ( 'NONE',  ( 8.442910196168311288, 4.355403765523574222, 1.898862081921442790 ) ) ;
#8878 = UNCERTAINTY_MEASURE_WITH_UNIT (LENGTH_MEASURE( 1.000000000000000082E-05 ), #8772, 'distance_accuracy_value', 'NONE');
#8879 = CARTESIAN_POINT ( 'NONE',  ( -10.24623928997352351, -10.06191849875416899, 44.50404056962644006 ) ) ;
#8880 = CARTESIAN_POINT ( 'NONE',  ( -5.284464991282755264, 15.10213328493384743, 18.42857142857143415 ) ) ;
#8881 = CARTESIAN_POINT ( 'NONE',  ( 11.92174236212692229, 7.340858601238088532, 35.71832628391214115 ) ) ;
#8882 = CARTESIAN_POINT ( 'NONE',  ( -7.448449071214644945, -11.85413878919601771, 4.285714285714288252 ) ) ;
#8883 = CARTESIAN_POINT ( 'NONE',  ( 8.464561979789474222, 4.312909747525755400, 15.90000000000002522 ) ) ;
#8884 = CARTESIAN_POINT ( 'NONE',  ( -9.859792900771106261, 4.967534682030611215, 12.84886208192143009 ) ) ;
#8885 = ORIENTED_EDGE ( 'NONE', *, *, #3292, .F. ) ;
#8886 = CARTESIAN_POINT ( 'NONE',  ( -7.448449071214644945, -11.85413878919601771, 16.28571428571428470 ) ) ;
#8887 = ORIENTED_EDGE ( 'NONE', *, *, #5443, .T. ) ;
#8888 = DIRECTION ( 'NONE',  ( 0.7056782240951884333, 0.7056782240951970930, 0.06353336191096713159 ) ) ;
#8889 =( GEOMETRIC_REPRESENTATION_CONTEXT ( 3 ) GLOBAL_UNCERTAINTY_ASSIGNED_CONTEXT ( ( #4320 ) ) GLOBAL_UNIT_ASSIGNED_CONTEXT ( ( #2333, #6915, #6242 ) ) REPRESENTATION_CONTEXT ( 'NONE', 'WORKASPACE' ) );
#8890 = CARTESIAN_POINT ( 'NONE',  ( 15.10213328493390783, -5.284464991282587398, 20.57142857142857295 ) ) ;
#8891 = CARTESIAN_POINT ( 'NONE',  ( 5.297344310588354865, 15.53355953199867301, 33.06738800180213644 ) ) ;
#8892 = CARTESIAN_POINT ( 'NONE',  ( 4.766900247265192903, 9.355568503977911732, 9.599999999999997868 ) ) ;
#8893 = CARTESIAN_POINT ( 'NONE',  ( -10.90442828429183919, -1.727091770866654663, 17.55000000000002913 ) ) ;
#8894 = CARTESIAN_POINT ( 'NONE',  ( -1.567502665446231180, -13.91197093850540334, 15.85714285714286120 ) ) ;
#8895 = VERTEX_POINT ( 'NONE', #7472 ) ;
#8896 = ORIENTED_EDGE ( 'NONE', *, *, #1783, .T. ) ;
#8897 = CARTESIAN_POINT ( 'NONE',  ( -10.90442828429184274, -1.727091770866655107, 11.54999999999998295 ) ) ;
#8898 = CARTESIAN_POINT ( 'NONE',  ( 0.000000000000000000, 0.000000000000000000, 0.000000000000000000 ) ) ;
#8899 = CARTESIAN_POINT ( 'NONE',  ( 10.06191849875406064, 10.24623928997363187, 39.49595943037357415 ) ) ;
#8900 = CARTESIAN_POINT ( 'NONE',  ( 7.390897758835871301, -7.458344646081624063, 12.50113791807859265 ) ) ;
#8901 = CARTESIAN_POINT ( 'NONE',  ( 7.842167650704563897, 7.771249796623202144, -0.2488620819214366897 ) ) ;
#8902 = PLANE ( 'NONE',  #6267 ) ;
#8903 = CARTESIAN_POINT ( 'NONE',  ( 1.693770420379222319, 13.89774397934251837, 16.86118342676929061 ) ) ;
#8904 = APPLICATION_CONTEXT ( 'automotive_design' ) ;
#8905 = CARTESIAN_POINT ( 'NONE',  ( 4.503970704919991519, -13.25633410266674517, 19.43261199819785645 ) ) ;
#8906 = PLANE ( 'NONE',  #782 ) ;
#8907 = SHAPE_REPRESENTATION ( 'piston', ( #3995 ), #9548 ) ;
#8908 = CARTESIAN_POINT ( 'NONE',  ( 13.96533075980324234, -8.621071003556521006, 4.781673716087850856 ) ) ;
#8909 = CARTESIAN_POINT ( 'NONE',  ( -166.6500000000000341, -1.532656777835077474E-15, 13.00000000000000355 ) ) ;
#8910 = CARTESIAN_POINT ( 'NONE',  ( -163.0672239440268356, -0.9520965995333376952, 14.97031403060969446 ) ) ;
#8911 = CARTESIAN_POINT ( 'NONE',  ( 4.490180821391514421, -8.922933199037132113, 6.651137918078563693 ) ) ;
#8912 = CARTESIAN_POINT ( 'NONE',  ( -4.312909747525649706, -8.464561979789499091, 8.099999999999996092 ) ) ;
#8913 = CARTESIAN_POINT ( 'NONE',  ( -162.8500000000000796, 0.1404462806920659668, 13.00000000000000533 ) ) ;
#8914 = CARTESIAN_POINT ( 'NONE',  ( -7.448449071214644945, -11.85413878919601771, 34.28571428571428470 ) ) ;
#8915 = CARTESIAN_POINT ( 'NONE',  ( 11.22385875690717683, -11.40355824106234373, 43.00404056962644717 ) ) ;
#8916 = ORIENTED_EDGE ( 'NONE', *, *, #4549, .F. ) ;
#8917 = AXIS2_PLACEMENT_3D ( 'NONE', #10183, #2427, #887 ) ;
#8918 = CARTESIAN_POINT ( 'NONE',  ( 11.60466159355862104, 11.60466159355875071, 31.50000000000001421 ) ) ;
#8919 = CARTESIAN_POINT ( 'NONE',  ( 3.856535827843035946, 14.61332904867485816, 3.589645083303631449E-17 ) ) ;
#8920 = CARTESIAN_POINT ( 'NONE',  ( 8.512513224245308763, 13.54758718765259040, 19.28571428571428825 ) ) ;
#8921 = EDGE_CURVE ( 'NONE', #273, #8732, #5613, .T. ) ;
#8922 = SURFACE_SIDE_STYLE ('',( #1989 ) ) ;
#8923 = CARTESIAN_POINT ( 'NONE',  ( -7.063212654743466601, -7.063212654743534991, 2.249999999999986233 ) ) ;
#8924 = CARTESIAN_POINT ( 'NONE',  ( 9.333916720356675967, 4.809394265263126300, 16.89886208192141126 ) ) ;
#8925 = CARTESIAN_POINT ( 'NONE',  ( -1.707986654103994528, 16.32287076676380266, 10.64689771248357886 ) ) ;
#8926 = AXIS2_PLACEMENT_3D ( 'NONE', #9751, #4211, #6475 ) ;
#8927 = CARTESIAN_POINT ( 'NONE',  ( -8.512513224245306986, -13.54758718765259218, 28.28571428571428825 ) ) ;
#8928 = VECTOR ( 'NONE', #4581, 1000.000000000000000 ) ;
#8929 = CIRCLE ( 'NONE', #7924, 1.000000000000000888 ) ;
#8930 = DIRECTION ( 'NONE',  ( 0.000000000000000000, 0.000000000000000000, 1.000000000000000000 ) ) ;
#8931 = CARTESIAN_POINT ( 'NONE',  ( 15.53355953199861794, 5.297344310588528060, -0.06738800180213055935 ) ) ;
#8932 = CARTESIAN_POINT ( 'NONE',  ( 15.10213328493390783, -5.284464991282587398, 38.57142857142857650 ) ) ;
#8933 = CARTESIAN_POINT ( 'NONE',  ( 4.623906867372411078, -13.21436662431711717, 15.42857142857143060 ) ) ;
#8934 = CARTESIAN_POINT ( 'NONE',  ( -8.900167166472160218, 4.534861676072235781, 17.85000000000001918 ) ) ;
#8935 = CARTESIAN_POINT ( 'NONE',  ( 9.859792900771104485, -4.967534682030588122, 11.34886208192143364 ) ) ;
#8936 = ORIENTED_EDGE ( 'NONE', *, *, #10020, .F. ) ;
#8937 = CARTESIAN_POINT ( 'NONE',  ( -10.15407889436378852, -10.15407889436390576, 16.50000000000000000 ) ) ;
#8938 = CIRCLE ( 'NONE', #1676, 15.99999999999999289 ) ;
#8939 = EDGE_LOOP ( 'NONE', ( #8896, #5418 ) ) ;
#8940 = MECHANICAL_DESIGN_GEOMETRIC_PRESENTATION_REPRESENTATION (  '', ( #3152 ), #7940 ) ;
#8941 = CIRCLE ( 'NONE', #2988, 18.00000000000000000 ) ;
#8942 = AXIS2_PLACEMENT_3D ( 'NONE', #5881, #2635, #5932 ) ;
#8943 = CARTESIAN_POINT ( 'NONE',  ( 15.49051278174637858, 5.420364854932174126, 25.92857142857143060 ) ) ;
#8944 = CARTESIAN_POINT ( 'NONE',  ( -5.404401153735176599, 15.06016580658422477, 32.42453085894499054 ) ) ;
#8945 = CARTESIAN_POINT ( 'NONE',  ( -4.766900247265192014, -9.355568503977867323, 11.09999999999999787 ) ) ;
#8946 = CARTESIAN_POINT ( 'NONE',  ( -10.37072757624895836, 1.642561882922380034, 11.69999999999998863 ) ) ;
#8947 = CARTESIAN_POINT ( 'NONE',  ( 10.15407889436379030, 10.15407889436390221, 13.50000000000000355 ) ) ;
#8948 = MECHANICAL_DESIGN_GEOMETRIC_PRESENTATION_REPRESENTATION (  '', ( #5948 ), #1680 ) ;
#8949 = CARTESIAN_POINT ( 'NONE',  ( 1.441234910513245149, 13.92619789766829008, 26.85310228751642470 ) ) ;
#8950 = LINE ( 'NONE', #5013, #7714 ) ;
#8951 = FACE_OUTER_BOUND ( 'NONE', #2074, .T. ) ;
#8952 = COLOUR_RGB ( '', 0.09019608, 0.27058824, 0.51372549) ;
#8953 = EDGE_CURVE ( 'NONE', #5915, #3726, #3370, .T. ) ;
#8954 = CARTESIAN_POINT ( 'NONE',  ( -13.51115193377584589, -4.865839792409295761, 42.92453085894499054 ) ) ;
#8955 = AXIS2_PLACEMENT_3D ( 'NONE', #4364, #1987, #10049 ) ;
#8956 = CARTESIAN_POINT ( 'NONE',  ( 1.727091770866550968, 10.90442828429187294, 0.4499999999999856337 ) ) ;
#8957 = CARTESIAN_POINT ( 'NONE',  ( -4.967534682030703586, 9.859792900771061852, 5.151137918078567246 ) ) ;
#8958 = ADVANCED_BREP_SHAPE_REPRESENTATION ( '', ( #7057, #3995 ), #3161 ) ;
#8959 = FACE_OUTER_BOUND ( 'NONE', #8405, .T. ) ;
#8960 = CARTESIAN_POINT ( 'NONE',  ( 9.809645194534072132, -9.989344678689256796, 19.00404056962642940 ) ) ;
#8961 = SURFACE_STYLE_FILL_AREA ( #8375 ) ;
#8962 = CARTESIAN_POINT ( 'NONE',  ( -13.92619789766827054, -1.441234910513399470, 21.14689771248358241 ) ) ;
#8963 = CARTESIAN_POINT ( 'NONE',  ( 4.766900247265192903, 9.355568503977902850, 3.599999999999992095 ) ) ;
#8964 = CARTESIAN_POINT ( 'NONE',  ( 1.665163862719847732, 15.91362231745477374, 44.85310228751641404 ) ) ;
#8965 = ORIENTED_EDGE ( 'NONE', *, *, #1944, .T. ) ;
#8966 = DIRECTION ( 'NONE',  ( 6.162975822039153635E-32, 0.5000000000000011102, 0.8660254037844379305 ) ) ;
#8967 = CARTESIAN_POINT ( 'NONE',  ( -1.967016585148659846, 16.29368510291087091, 8.638816573230704066 ) ) ;
#8968 = CARTESIAN_POINT ( 'NONE',  ( -168.0000000000000284, 11.00000000000000178, 1.347111479062088799E-15 ) ) ;
#8969 = CARTESIAN_POINT ( 'NONE',  ( -164.7164049854163181, -2.135816869796272943, 14.84719012526269388 ) ) ;
#8970 = EDGE_CURVE ( 'NONE', #9396, #10190, #833, .T. ) ;
#8971 = CARTESIAN_POINT ( 'NONE',  ( 8.877401133907127928, -4.579542530753017537, 3.351137918078579858 ) ) ;
#8972 = CARTESIAN_POINT ( 'NONE',  ( 1.562606840307832368, 9.865911304835510265, 12.44999999999995666 ) ) ;
#8973 = CIRCLE ( 'NONE', #5812, 16.00000000000000000 ) ;
#8974 = LINE ( 'NONE', #434, #5775 ) ;
#8975 = CARTESIAN_POINT ( 'NONE',  ( -16.29368510291090288, 1.967016585148476215, 39.36118342676930837 ) ) ;
#8976 = CARTESIAN_POINT ( 'NONE',  ( -4.623906867372410190, 13.21436662431711895, 30.42857142857143060 ) ) ;
#8977 = CARTESIAN_POINT ( 'NONE',  ( -12.15899005565164792, 7.639999817571651697, 35.78571428571429180 ) ) ;
#8978 = VERTEX_POINT ( 'NONE', #2489 ) ;
#8979 = CARTESIAN_POINT ( 'NONE',  ( -15.49051278174638036, -5.420364854932175902, 46.92857142857142350 ) ) ;
#8980 = CARTESIAN_POINT ( 'NONE',  ( 3.732286808396943822, 14.38075913893019653, -9.697396257098258182E-17 ) ) ;
#8981 = CARTESIAN_POINT ( 'NONE',  ( 15.89939535829187278, 1.791431617653015174, 20.14285714285714235 ) ) ;
#8982 = PRODUCT_DEFINITION_SHAPE ( 'NONE', 'NONE',  #10228 ) ;
#8983 = CARTESIAN_POINT ( 'NONE',  ( 4.270415729527831772, 8.486213763410697553, 7.598862081921438971 ) ) ;
#8984 = PRODUCT_DEFINITION_CONTEXT ( 'detailed design', #7182, 'design' ) ;
#8985 = CARTESIAN_POINT ( 'NONE',  ( 8.620103694221997515, 13.47998361472160767, 5.289754855340725648 ) ) ;
#8986 = CARTESIAN_POINT ( 'NONE',  ( 15.89939535829187278, 1.791431617653015174, 32.14285714285714590 ) ) ;
#8987 =( NAMED_UNIT ( * ) PLANE_ANGLE_UNIT ( ) SI_UNIT ( $, .RADIAN. ) );
#8988 = CARTESIAN_POINT ( 'NONE',  ( 11.69682198916835070, 11.51250119794901394, 5.504040569626439172 ) ) ;
#8989 = CARTESIAN_POINT ( 'NONE',  ( -4.623906867372410190, 13.21436662431711895, 6.428571428571429713 ) ) ;
#8990 = CARTESIAN_POINT ( 'NONE',  ( 1.486127417882244783, -9.383039235653791721, 16.80000000000003624 ) ) ;
#8991 = CARTESIAN_POINT ( 'NONE',  ( 7.458344646081711105, -7.390897758835778930, 8.498862081921462419 ) ) ;
#8992 = EDGE_LOOP ( 'NONE', ( #5012, #3958 ) ) ;
#8993 = CARTESIAN_POINT ( 'NONE',  ( -13.21436662431716869, 4.623906867372262752, 11.57142857142857295 ) ) ;
#8994 = EDGE_CURVE ( 'NONE', #4164, #4139, #1620, .T. ) ;
#8995 = VERTEX_POINT ( 'NONE', #3321 ) ;
#8996 = VECTOR ( 'NONE', #4235, 1000.000000000000000 ) ;
#8997 = CARTESIAN_POINT ( 'NONE',  ( 1.837501619626329630, -16.30827793483733501, 33.64285714285714590 ) ) ;
#8998 = CARTESIAN_POINT ( 'NONE',  ( -5.404401153735176599, 15.06016580658422477, 50.42453085894499765 ) ) ;
#8999 = CARTESIAN_POINT ( 'NONE',  ( 9.837026868206066865, -5.012215536711391195, 10.35000000000002274 ) ) ;
#9000 = CARTESIAN_POINT ( 'NONE',  ( 11.85413878919593422, 7.448449071214774619, 13.71428571428571352 ) ) ;
#9001 = CARTESIAN_POINT ( 'NONE',  ( 12.22833218042443271, -7.529642458189144349, 28.78167371608785174 ) ) ;
#9002 = DIRECTION ( 'NONE',  ( -1.000000000000000000, -0.000000000000000000, -0.000000000000000000 ) ) ;
#9003 = CARTESIAN_POINT ( 'NONE',  ( 0.6500995950961804271, 14.01729557978340956, 48.73000000000002530 ) ) ;
#9004 = CARTESIAN_POINT ( 'NONE',  ( -13.25633410266679313, 4.503970704919840529, 37.56738800180213644 ) ) ;
#9005 = CARTESIAN_POINT ( 'NONE',  ( 10.36326688006723984, -1.689666864740212215, 12.20113791807854398 ) ) ;
#9006 = CARTESIAN_POINT ( 'NONE',  ( -9.377220287598998283, -4.724406229267462898, 4.401137918078569022 ) ) ;
#9007 = DIRECTION ( 'NONE',  ( 1.000000000000000000, 4.755747939841215952E-17, -0.000000000000000000 ) ) ;
#9008 = CARTESIAN_POINT ( 'NONE',  ( 7.529642458189280241, -12.22833218042435099, 13.21832628391215181 ) ) ;
#9009 = SURFACE_STYLE_USAGE ( .BOTH. , #374 ) ;
#9010 = EDGE_CURVE ( 'NONE', #557, #3401, #6458, .T. ) ;
#9011 = CARTESIAN_POINT ( 'NONE',  ( -7.529642458189277576, 12.22833218042435455, 28.21832628391215181 ) ) ;
#9012 = CARTESIAN_POINT ( 'NONE',  ( 9.355568503977840678, 4.766900247265305701, 9.900000000000019895 ) ) ;
#9013 = CARTESIAN_POINT ( 'NONE',  ( 15.44746603149413922, 5.543385399275817527, 39.92453085894499054 ) ) ;
#9014 = CARTESIAN_POINT ( 'NONE',  ( -5.986002070941133901, -13.58603705635637304, 0.000000000000000000 ) ) ;
#9015 = CARTESIAN_POINT ( 'NONE',  ( 8.512513224245308763, 13.54758718765259040, 19.28571428571428825 ) ) ;
#9016 = CARTESIAN_POINT ( 'NONE',  ( 15.88516839912898071, 1.917699372586004092, 10.13881657323070762 ) ) ;
#9017 = DIRECTION ( 'NONE',  ( -0.000000000000000000, 0.000000000000000000, -1.000000000000000000 ) ) ;
#9018 = EDGE_CURVE ( 'NONE', #9666, #8978, #6588, .T. ) ;
#9019 = CARTESIAN_POINT ( 'NONE',  ( -8.486213763410637156, -4.270415729527911708, 1.401137918078568134 ) ) ;
#9020 = CARTESIAN_POINT ( 'NONE',  ( -8.464561979789474222, -4.312909747525729642, 14.39999999999996838 ) ) ;
#9021 = CARTESIAN_POINT ( 'NONE',  ( 2.000000000000001776, 1.773042676681366281, 0.000000000000000000 ) ) ;
#9022 = CARTESIAN_POINT ( 'NONE',  ( -8.620103694221995738, -13.47998361472161299, 38.28975485534072476 ) ) ;
#9023 = CARTESIAN_POINT ( 'NONE',  ( -11.85413878919593422, -7.448449071214776396, 34.71428571428571530 ) ) ;
#9024 = EDGE_LOOP ( 'NONE', ( #3773, #7177 ) ) ;
#9025 = CARTESIAN_POINT ( 'NONE',  ( -1.791431617652833763, -15.89939535829188877, 45.85714285714286120 ) ) ;
#9026 = CARTESIAN_POINT ( 'NONE',  ( -43.00000000000002842, 6.933347799794049071E-30, -9.629649721936179265E-31 ) ) ;
#9027 = CARTESIAN_POINT ( 'NONE',  ( -11.31370849898482156, 11.31370849898469544, 11.99999999999999645 ) ) ;
#9028 = CARTESIAN_POINT ( 'NONE',  ( 4.246973736992224246, -14.10948682827615919, -1.270000000000007123 ) ) ;
#9029 = CARTESIAN_POINT ( 'NONE',  ( 6.751237864895159646, -6.683790977649239906, 20.49886208192143400 ) ) ;
#9030 = CARTESIAN_POINT ( 'NONE',  ( 4.270415729527831772, 8.486213763410694000, 10.59886208192144075 ) ) ;
#9031 = CARTESIAN_POINT ( 'NONE',  ( -8.621071003556675549, 13.96533075980314642, 4.218326283912150032 ) ) ;
#9032 = CARTESIAN_POINT ( 'NONE',  ( 11.31370849898482334, -11.31370849898469366, 27.00000000000000355 ) ) ;
#9033 = CIRCLE ( 'NONE', #4741, 1.816100000000000270 ) ;
#9034 = CARTESIAN_POINT ( 'NONE',  ( -14.26974319298268767, 1.607813917172874696, 47.35714285714286120 ) ) ;
#9035 = CARTESIAN_POINT ( 'NONE',  ( 5.543385399275644332, 15.44746603149420494, 5.075469141055008571 ) ) ;
#9036 = CARTESIAN_POINT ( 'NONE',  ( 4.623906867372411078, -13.21436662431711717, 27.42857142857143060 ) ) ;
#9037 = CARTESIAN_POINT ( 'NONE',  ( -16.00000000000000000, 0.000000000000000000, 20.00000000000001776 ) ) ;
#9038 = PLANE ( 'NONE',  #6104 ) ;
#9039 = EDGE_LOOP ( 'NONE', ( #2532, #4329, #5140, #1451 ) ) ;
#9040 = CARTESIAN_POINT ( 'NONE',  ( -13.55419868402807992, -4.742819248065651472, 10.92857142857142883 ) ) ;
#9041 = ORIENTED_EDGE ( 'NONE', *, *, #9306, .T. ) ;
#9042 = VECTOR ( 'NONE', #10127, 1000.000000000000000 ) ;
#9043 = CARTESIAN_POINT ( 'NONE',  ( -13.89598863503045933, 8.731428362939027465, 35.78571428571429180 ) ) ;
#9044 = CARTESIAN_POINT ( 'NONE',  ( 4.619798703721856192, 13.59724543428036725, 3.067388001802140884 ) ) ;
#9045 = CARTESIAN_POINT ( 'NONE',  ( -10.89658364409024749, -1.776620879821561694, 3.548862081921419609 ) ) ;
#9046 = PRODUCT_CONTEXT ( 'NONE', #1512, 'mechanical' ) ;
#9047 = CARTESIAN_POINT ( 'NONE',  ( -7.448449071214644945, -11.85413878919601771, 10.28571428571428648 ) ) ;
#9048 = ORIENTED_EDGE ( 'NONE', *, *, #10187, .T. ) ;
#9049 = CARTESIAN_POINT ( 'NONE',  ( -1.441234910513241818, -13.92619789766829008, 23.85310228751642825 ) ) ;
#9050 = MECHANICAL_DESIGN_GEOMETRIC_PRESENTATION_REPRESENTATION (  '', ( #7732 ), #1461 ) ;
#9051 = VERTEX_POINT ( 'NONE', #3165 ) ;
#9052 = PRESENTATION_STYLE_ASSIGNMENT (( #4285 ) ) ;
#9053 = LINE ( 'NONE', #3516, #5018 ) ;
#9054 = CARTESIAN_POINT ( 'NONE',  ( 4.270415729527831772, 8.486213763410688671, 1.598862081921434308 ) ) ;
#9055 = CARTESIAN_POINT ( 'NONE',  ( 10.15407889436379030, 10.15407889436390576, 1.500000000000003553 ) ) ;
#9056 = CARTESIAN_POINT ( 'NONE',  ( -1.727091770866549414, -10.90442828429184630, 1.949999999999996181 ) ) ;
#9057 = CARTESIAN_POINT ( 'NONE',  ( 10.91227292449344155, 1.677562661911773167, 6.051137918078538291 ) ) ;
#9058 = PRODUCT_DEFINITION_FORMATION_WITH_SPECIFIED_SOURCE ( 'ANY', '', #2773, .NOT_KNOWN. ) ;
#9059 = CARTESIAN_POINT ( 'NONE',  ( 4.200000000000009059, 2.694222958124178486E-16, 2.200000000000001066 ) ) ;
#9060 = CARTESIAN_POINT ( 'NONE',  ( -14.25515036105622890, 1.737328882695209575, 21.36118342676929771 ) ) ;
#9061 = CARTESIAN_POINT ( 'NONE',  ( -13.92619789766827054, -1.441234910513399470, 27.14689771248358241 ) ) ;
#9062 = CARTESIAN_POINT ( 'NONE',  ( 9.837026868206066865, -5.012215536711391195, 4.350000000000036948 ) ) ;
#9063 = CARTESIAN_POINT ( 'NONE',  ( -13.47998361472151174, -8.620103694222146729, 36.71024514465928235 ) ) ;
#9064 = CARTESIAN_POINT ( 'NONE',  ( -4.874503691416085971, 13.19452956797008802, 48.73000000000003951 ) ) ;
#9065 = CARTESIAN_POINT ( 'NONE',  ( -15.10213328493390961, 5.284464991282586510, 23.57142857142857650 ) ) ;
#9066 = DIRECTION ( 'NONE',  ( -6.162975822039154730E-33, -0.4999999999999991118, 0.8660254037844391517 ) ) ;
#9067 = CARTESIAN_POINT ( 'NONE',  ( -13.89774397934249706, -1.693770420379375974, 19.13881657323070584 ) ) ;
#9068 = CARTESIAN_POINT ( 'NONE',  ( 4.355403765523470305, 8.442910196168364578, 2.601137918078560762 ) ) ;
#9069 = CARTESIAN_POINT ( 'NONE',  ( 7.063212654743467489, 7.063212654743553642, 15.74999999999996803 ) ) ;
#9070 = CARTESIAN_POINT ( 'NONE',  ( -163.2907867177267462, 1.311749039217684709, 14.94298962415842880 ) ) ;
#9071 = CARTESIAN_POINT ( 'NONE',  ( -13.91197093850538380, -1.567502665446387278, 29.14285714285714235 ) ) ;
#9072 = CARTESIAN_POINT ( 'NONE',  ( -7.639999817571787588, 12.15899005565156266, 36.21428571428573662 ) ) ;
#9073 = VERTEX_POINT ( 'NONE', #6303 ) ;
#9074 = CARTESIAN_POINT ( 'NONE',  ( -2.030095817397326030, 15.65302214768666467, 5.081489463560611418E-16 ) ) ;
#9075 = CARTESIAN_POINT ( 'NONE',  ( 11.60466159355862104, 11.60466159355875071, 19.50000000000000355 ) ) ;
#9076 = CARTESIAN_POINT ( 'NONE',  ( 8.787954181158717404, -8.913453481710838844, -1.270000000000007123 ) ) ;
#9077 = DIRECTION ( 'NONE',  ( -1.000000000000000000, 4.575525868300071581E-16, 0.000000000000000000 ) ) ;
#9078 = DIRECTION ( 'NONE',  ( 0.000000000000000000, 1.000000000000000000, 0.000000000000000000 ) ) ;
#9079 = CARTESIAN_POINT ( 'NONE',  ( 6.751237864895159646, -6.683790977649233689, 14.49886208192142867 ) ) ;
#9080 = CARTESIAN_POINT ( 'NONE',  ( 7.027753727702739539, 7.098671581784288698, 7.748862081921418010 ) ) ;
#9081 = CARTESIAN_POINT ( 'NONE',  ( -15.06016580658428694, 5.404401153735006957, 3.575469141055005462 ) ) ;
#9082 = CARTESIAN_POINT ( 'NONE',  ( -5.420364854931999155, -15.49051278174644253, 28.07142857142857295 ) ) ;
#9083 = CARTESIAN_POINT ( 'NONE',  ( 0.000000000000000000, 0.000000000000000000, 68.00000000000000000 ) ) ;
#9084 = CARTESIAN_POINT ( 'NONE',  ( 8.620103694221997515, 13.47998361472160767, 5.289754855340725648 ) ) ;
#9085 = AXIS2_PLACEMENT_3D ( 'NONE', #6486, #248, #1901 ) ;
#9086 = CARTESIAN_POINT ( 'NONE',  ( -13.21436662431716869, 4.623906867372262752, 29.57142857142857650 ) ) ;
#9087 = DIRECTION ( 'NONE',  ( -1.000000000000000000, -0.000000000000000000, -0.000000000000000000 ) ) ;
#9088 = ORIENTED_EDGE ( 'NONE', *, *, #8842, .T. ) ;
#9089 = CARTESIAN_POINT ( 'NONE',  ( -11.85413878919593422, -7.448449071214776396, 16.71428571428571530 ) ) ;
#9090 = ORIENTED_EDGE ( 'NONE', *, *, #268, .T. ) ;
#9091 = CARTESIAN_POINT ( 'NONE',  ( 11.60466159355861926, 11.60466159355874716, 37.50000000000001421 ) ) ;
#9092 = VECTOR ( 'NONE', #7884, 1000.000000000000000 ) ;
#9093 = AXIS2_PLACEMENT_3D ( 'NONE', #4883, #8028, #7357 ) ;
#9094 = CARTESIAN_POINT ( 'NONE',  ( -15.44746603149413922, -5.543385399275820191, 48.92453085894499054 ) ) ;
#9095 = CARTESIAN_POINT ( 'NONE',  ( -4.766900247265192014, -9.355568503977876205, 14.10000000000000142 ) ) ;
#9096 = SHAPE_DEFINITION_REPRESENTATION ( #1215, #1047 ) ;
#9097 = CARTESIAN_POINT ( 'NONE',  ( -13.91197093850538380, -1.567502665446387278, 11.14285714285714235 ) ) ;
#9098 = CIRCLE ( 'NONE', #5934, 13.00000000000001421 ) ;
#9099 = AXIS2_PLACEMENT_3D ( 'NONE', #9289, #653, #2248 ) ;
#9100 = CIRCLE ( 'NONE', #3154, 3.632200000000000539 ) ;
#9101 = ORIENTED_EDGE ( 'NONE', *, *, #5165, .T. ) ;
#9102 = CARTESIAN_POINT ( 'NONE',  ( 11.78653521626494793, 7.556039541191463371, 21.71024514465928235 ) ) ;
#9103 = VERTEX_POINT ( 'NONE', #2390 ) ;
#9104 = CARTESIAN_POINT ( 'NONE',  ( -166.5657114886604120, 0.5317309469415117951, 12.98950588154195351 ) ) ;
#9105 =( REPRESENTATION_RELATIONSHIP ('NONE','NONE', #58, #3956 ) REPRESENTATION_RELATIONSHIP_WITH_TRANSFORMATION ( #1548 )SHAPE_REPRESENTATION_RELATIONSHIP( ) );
#9106 = CARTESIAN_POINT ( 'NONE',  ( -7.771249796623103556, -7.842167650704634063, 18.24886208192143044 ) ) ;
#9107 = CARTESIAN_POINT ( 'NONE',  ( -9.899494936611716867, 9.899494936611610285, 0.000000000000000000 ) ) ;
#9108 = CARTESIAN_POINT ( 'NONE',  ( -1.727091770866549414, -10.90442828429185695, 4.950000000000017053 ) ) ;
#9109 = CARTESIAN_POINT ( 'NONE',  ( 4.967534682030706250, -9.859792900771036983, 6.651137918078563693 ) ) ;
#9110 = CARTESIAN_POINT ( 'NONE',  ( -158.0000000000000284, -18.00000000000001066, 0.000000000000000000 ) ) ;
#9111 = CARTESIAN_POINT ( 'NONE',  ( 1.478298951650704351, -14.28433602490913579, 25.64689771248357886 ) ) ;
#9112 = SURFACE_STYLE_FILL_AREA ( #9789 ) ;
#9113 = ADVANCED_FACE ( 'NONE', ( #9937 ), #9880, .F. ) ;
#9114 = CARTESIAN_POINT ( 'NONE',  ( 7.806708723663831506, 7.806708723663930982, 6.749999999999960032 ) ) ;
#9115 = CARTESIAN_POINT ( 'NONE',  ( 13.47998361472151529, 8.620103694222146729, 39.71024514465927524 ) ) ;
#9116 = VERTEX_POINT ( 'NONE', #9110 ) ;
#9117 = CARTESIAN_POINT ( 'NONE',  ( -2.607279028132698961, 15.78019693191412287, 48.73000000000003951 ) ) ;
#9118 = CARTESIAN_POINT ( 'NONE',  ( -11.60466159355861926, -11.60466159355875249, 22.50000000000000000 ) ) ;
#9119 = EDGE_CURVE ( 'NONE', #3374, #4587, #2164, .T. ) ;
#9120 = CARTESIAN_POINT ( 'NONE',  ( -68.00000000000002842, 0.000000000000000000, 0.000000000000000000 ) ) ;
#9121 = EDGE_CURVE ( 'NONE', #8205, #7530, #514, .T. ) ;
#9122 = CARTESIAN_POINT ( 'NONE',  ( 13.51115193377584589, 4.865839792409294873, 9.924530858944988765 ) ) ;
#9123 = CARTESIAN_POINT ( 'NONE',  ( 1.439022436064387511, -9.390499931835510239, 15.80113791807855961 ) ) ;
#9124 = CARTESIAN_POINT ( 'NONE',  ( -1.439022436064386845, 9.390499931835535108, -0.6988620819214501623 ) ) ;
#9125 = CARTESIAN_POINT ( 'NONE',  ( -163.5800396265123595, 1.620586088255114188, 14.91253992662286976 ) ) ;
#9126 = CARTESIAN_POINT ( 'NONE',  ( 11.22385875690717683, -11.40355824106234373, 37.00404056962644006 ) ) ;
#9127 = CARTESIAN_POINT ( 'NONE',  ( 8.784089738577305795, 11.01490013464600892, 49.39149694378009769 ) ) ;
#9128 = CARTESIAN_POINT ( 'NONE',  ( 4.623906867372411078, -13.21436662431711717, 39.42857142857143060 ) ) ;
#9129 = ORIENTED_EDGE ( 'NONE', *, *, #9774, .T. ) ;
#9130 = CARTESIAN_POINT ( 'NONE',  ( -13.89598863503046111, 8.731428362939027465, 41.78571428571430602 ) ) ;
#9131 = DIRECTION ( 'NONE',  ( 0.000000000000000000, 6.938893903907221444E-18, 1.000000000000000000 ) ) ;
#9132 = CARTESIAN_POINT ( 'NONE',  ( -8.512513224245306986, -13.54758718765259218, 28.28571428571428825 ) ) ;
#9133 = PLANE ( 'NONE',  #369 ) ;
#9134 = FACE_OUTER_BOUND ( 'NONE', #6962, .T. ) ;
#9135 = DIRECTION ( 'NONE',  ( -1.000000000000000000, -0.000000000000000000, -0.000000000000000000 ) ) ;
#9136 = CARTESIAN_POINT ( 'NONE',  ( 8.464561979789474222, 4.312909747525755400, 6.899999999999961275 ) ) ;
#9137 = CARTESIAN_POINT ( 'NONE',  ( 1.533232399700100945, -9.375578539472073203, 11.79886208192143471 ) ) ;
#9138 = CARTESIAN_POINT ( 'NONE',  ( -10.37072757624895836, 1.642561882922380034, 14.69999999999999041 ) ) ;
#9139 = CARTESIAN_POINT ( 'NONE',  ( 15.91362231745475597, 1.665163862720026255, 12.14689771248358063 ) ) ;
#9140 = CARTESIAN_POINT ( 'NONE',  ( 15.49051278174638036, 5.420364854932175014, 31.92857142857143415 ) ) ;
#9141 = CARTESIAN_POINT ( 'NONE',  ( -1.917699372585823570, -15.88516839912900558, 1.861183426769295490 ) ) ;
#9142 = ADVANCED_FACE ( 'NONE', ( #5984 ), #1243, .F. ) ;
#9143 = CARTESIAN_POINT ( 'NONE',  ( 8.731428362939190890, -13.89598863503036164, 9.214285714285717077 ) ) ;
#9144 = CARTESIAN_POINT ( 'NONE',  ( 15.89939535829187278, 1.791431617653015174, 44.14285714285714590 ) ) ;
#9145 = VERTEX_POINT ( 'NONE', #5019 ) ;
#9146 = CARTESIAN_POINT ( 'NONE',  ( 7.806708723663831506, 7.806708723663925653, 15.74999999999996803 ) ) ;
#9147 = EDGE_LOOP ( 'NONE', ( #3650, #4259 ) ) ;
#9148 = CARTESIAN_POINT ( 'NONE',  ( -15.10213328493390961, 5.284464991282586510, 29.57142857142857650 ) ) ;
#9149 = CARTESIAN_POINT ( 'NONE',  ( -11.40355824106246807, 11.22385875690704715, 49.99595943037357415 ) ) ;
#9150 = CARTESIAN_POINT ( 'NONE',  ( -9.859792900771106261, 4.967534682030611215, 3.848862081921410105 ) ) ;
#9151 = PRODUCT ( 'main spring', 'main spring', '', ( #8361 ) ) ;
#9152 = CARTESIAN_POINT ( 'NONE',  ( -11.85413878919593422, -7.448449071214776396, 28.71428571428571530 ) ) ;
#9153 = CARTESIAN_POINT ( 'NONE',  ( -1.737328882695368115, 14.25515036105620581, 26.63881657323070939 ) ) ;
#9154 = AXIS2_PLACEMENT_3D ( 'NONE', #1248, #4454, #7553 ) ;
#9155 = ORIENTED_EDGE ( 'NONE', *, *, #8807, .T. ) ;
#9156 = CARTESIAN_POINT ( 'NONE',  ( 9.355568503977840678, 4.766900247265305701, 18.90000000000002700 ) ) ;
#9157 = EDGE_CURVE ( 'NONE', #913, #7562, #4478, .T. ) ;
#9158 = CARTESIAN_POINT ( 'NONE',  ( -163.3500000000000512, -1.154202410357457390E-14, 13.00000000000000355 ) ) ;
#9159 = CARTESIAN_POINT ( 'NONE',  ( -4.724406229267374968, -9.377220287599040915, 18.09886208192144252 ) ) ;
#9160 = CARTESIAN_POINT ( 'NONE',  ( -14.28433602490915000, 1.478298951650542481, 49.35310228751642114 ) ) ;
#9161 = CARTESIAN_POINT ( 'NONE',  ( 5.012215536711511987, -9.837026868205999364, 1.650000000000006128 ) ) ;
#9162 = CARTESIAN_POINT ( 'NONE',  ( 1.776620879821457333, 10.89658364409027236, 14.45113791807853509 ) ) ;
#9163 = FACE_BOUND ( 'NONE', #9332, .T. ) ;
#9164 = CARTESIAN_POINT ( 'NONE',  ( -13.92619789766827054, -1.441234910513399470, 33.14689771248357886 ) ) ;
#9165 = DIRECTION ( 'NONE',  ( 1.000000000000000000, 0.000000000000000000, 0.000000000000000000 ) ) ;
#9166 = ORIENTED_EDGE ( 'NONE', *, *, #3129, .F. ) ;
#9167 = CARTESIAN_POINT ( 'NONE',  ( -10.37072757624895836, 1.642561882922381145, 5.700000000000038369 ) ) ;
#9168 = EDGE_LOOP ( 'NONE', ( #5406, #5101, #9676, #4700 ) ) ;
#9169 = CARTESIAN_POINT ( 'NONE',  ( -13.06814903599441280, 7.205911594201809045, 48.73000000000001108 ) ) ;
#9170 = CARTESIAN_POINT ( 'NONE',  ( 11.60466159355862104, 11.60466159355875071, 25.50000000000000711 ) ) ;
#9171 = DIRECTION ( 'NONE',  ( 1.000000000000000000, 0.000000000000000000, 0.000000000000000000 ) ) ;
#9172 = CARTESIAN_POINT ( 'NONE',  ( -12.22833218042443271, 7.529642458189139909, 13.78167371608785174 ) ) ;
#9173 = CARTESIAN_POINT ( 'NONE',  ( 4.355403765523470305, 8.442910196168369907, 17.60113791807856742 ) ) ;
#9174 = CARTESIAN_POINT ( 'NONE',  ( -9.383039235653820143, 1.486127417882154411, 11.69999999999998863 ) ) ;
#9175 = PLANE ( 'NONE',  #5454 ) ;
#9176 = CARTESIAN_POINT ( 'NONE',  ( 7.639999817571789364, -12.15899005565156266, 39.21428571428571530 ) ) ;
#9177 = CARTESIAN_POINT ( 'NONE',  ( -7.639999817571787588, 12.15899005565156266, 42.21428571428572241 ) ) ;
#9178 = EDGE_LOOP ( 'NONE', ( #3598, #9997, #726, #4312 ) ) ;
#9179 = CARTESIAN_POINT ( 'NONE',  ( -1.791431617652833763, -15.89939535829188877, 39.85714285714286120 ) ) ;
#9180 = CARTESIAN_POINT ( 'NONE',  ( 0.5828906444166439549, 15.62646852646394713, 9.306676823330757431E-17 ) ) ;
#9181 = CARTESIAN_POINT ( 'NONE',  ( -8.512513224245306986, -13.54758718765259218, 34.28571428571428470 ) ) ;
#9182 = CARTESIAN_POINT ( 'NONE',  ( -1.925929944387235853E-31, -1.018491042385001544, -1.270000000000007123 ) ) ;
#9183 =( NAMED_UNIT ( * ) SI_UNIT ( $, .STERADIAN. ) SOLID_ANGLE_UNIT ( ) );
#9184 = CARTESIAN_POINT ( 'NONE',  ( -10.37072757624895836, 1.642561882922380923, 2.699999999999980194 ) ) ;
#9185 = CARTESIAN_POINT ( 'NONE',  ( 4.312909747525650594, 8.464561979789541724, 6.599999999999994316 ) ) ;
#9186 = CARTESIAN_POINT ( 'NONE',  ( -8.442910196168309511, -4.355403765523544024, 12.39886208192140948 ) ) ;
#9187 = CARTESIAN_POINT ( 'NONE',  ( 10.37072757624895836, -1.642561882922355831, 19.19999999999999574 ) ) ;
#9188 = CARTESIAN_POINT ( 'NONE',  ( -15.91362231745475597, -1.665163862720028254, 21.14689771248358241 ) ) ;
#9189 = CARTESIAN_POINT ( 'NONE',  ( -5.284464991282755264, 15.10213328493384743, 42.42857142857143060 ) ) ;
#9190 = CARTESIAN_POINT ( 'NONE',  ( -13.61519076058348254, -8.404922754268771001, 20.71832628391214826 ) ) ;
#9191 = CARTESIAN_POINT ( 'NONE',  ( -7.639999817571787588, 12.15899005565156266, 24.21428571428571530 ) ) ;
#9192 = CARTESIAN_POINT ( 'NONE',  ( 13.54758718765249803, 8.512513224245457977, 1.714285714285716855 ) ) ;
#9193 = CARTESIAN_POINT ( 'NONE',  ( -8.512513224245306986, -13.54758718765259218, 40.28571428571428470 ) ) ;
#9194 = VERTEX_POINT ( 'NONE', #2018 ) ;
#9195 = CARTESIAN_POINT ( 'NONE',  ( 1.727091770866550968, 10.90442828429186761, 18.44999999999999218 ) ) ;
#9196 = ORIENTED_EDGE ( 'NONE', *, *, #2389, .T. ) ;
#9197 = CARTESIAN_POINT ( 'NONE',  ( 5.284464991282756152, -15.10213328493384743, 39.42857142857143060 ) ) ;
#9198 = CARTESIAN_POINT ( 'NONE',  ( -10.06191849875405531, -10.24623928997363542, 6.495959430373559051 ) ) ;
#9199 = CARTESIAN_POINT ( 'NONE',  ( -7.806708723663830618, -7.806708723663902560, 14.25000000000001243 ) ) ;
#9200 = CARTESIAN_POINT ( 'NONE',  ( 11.60466159355862104, 11.60466159355875071, 7.500000000000005329 ) ) ;
#9201 = DIRECTION ( 'NONE',  ( 0.000000000000000000, 0.000000000000000000, 1.000000000000000000 ) ) ;
#9202 = CARTESIAN_POINT ( 'NONE',  ( 1.607813917173037899, -14.26974319298267169, 21.64285714285714590 ) ) ;
#9203 = AXIS2_PLACEMENT_3D ( 'NONE', #9537, #5590, #4101 ) ;
#9204 = CARTESIAN_POINT ( 'NONE',  ( -11.78653521626494793, -7.556039541191465148, 36.71024514465928235 ) ) ;
#9205 = ORIENTED_EDGE ( 'NONE', *, *, #3669, .T. ) ;
#9206 = FACE_OUTER_BOUND ( 'NONE', #3714, .T. ) ;
#9207 = CARTESIAN_POINT ( 'NONE',  ( 15.88516839912898071, 1.917699372586004092, 28.13881657323070939 ) ) ;
#9208 = DIRECTION ( 'NONE',  ( 0.000000000000000000, 6.938893903907220674E-18, 1.000000000000000000 ) ) ;
#9209 = CARTESIAN_POINT ( 'NONE',  ( 7.771249796623105333, 7.842167650704658932, 19.74886208192143044 ) ) ;
#9210 = CARTESIAN_POINT ( 'NONE',  ( 7.806708723663831506, 7.806708723663925653, 9.749999999999982236 ) ) ;
#9211 = CARTESIAN_POINT ( 'NONE',  ( -10.91227292449344155, -1.677562661911747632, 16.55113791807855605 ) ) ;
#9212 = DIRECTION ( 'NONE',  ( -1.000000000000000000, -1.387778780781445676E-16, -0.000000000000000000 ) ) ;
#9213 = CARTESIAN_POINT ( 'NONE',  ( 4.766900247265192903, 9.355568503977902850, 15.60000000000000320 ) ) ;
#9214 = CARTESIAN_POINT ( 'NONE',  ( -13.47998361472151174, -8.620103694222146729, 48.71024514465926814 ) ) ;
#9215 = CARTESIAN_POINT ( 'NONE',  ( -5.012215536711508435, 9.837026868206027785, 0.1499999999999952482 ) ) ;
#9216 = DIRECTION ( 'NONE',  ( 1.000000000000000000, -4.575525868300071581E-16, -0.000000000000000000 ) ) ;
#9217 = CARTESIAN_POINT ( 'NONE',  ( 9.989344678689365153, -9.809645194533958446, 22.99595943037356705 ) ) ;
#9218 = CARTESIAN_POINT ( 'NONE',  ( 6.683790977649321619, -6.751237864895076157, 18.50113791807859087 ) ) ;
#9219 = CARTESIAN_POINT ( 'NONE',  ( -1.439022436064386845, 9.390499931835526226, 2.301137918078551614 ) ) ;
#9220 = DIRECTION ( 'NONE',  ( -1.000000000000000000, -0.000000000000000000, -0.000000000000000000 ) ) ;
#9221 = CARTESIAN_POINT ( 'NONE',  ( -13.55419868402807992, -4.742819248065651472, 40.92857142857145192 ) ) ;
#9222 = CARTESIAN_POINT ( 'NONE',  ( -4.503970704919988854, 13.25633410266674517, -1.567388001802134223 ) ) ;
#9223 = ORIENTED_EDGE ( 'NONE', *, *, #2119, .T. ) ;
#9224 = CARTESIAN_POINT ( 'NONE',  ( -15.44746603149413922, -5.543385399275820191, 6.924530858944994982 ) ) ;
#9225 = CARTESIAN_POINT ( 'NONE',  ( -7.071314881512976491, 14.31301652532476076, -4.192871190346640879E-15 ) ) ;
#9226 = CARTESIAN_POINT ( 'NONE',  ( 15.89939535829187278, 1.791431617653015174, 26.14285714285714590 ) ) ;
#9227 = DIRECTION ( 'NONE',  ( 0.000000000000000000, 6.338944243255235518E-49, -1.000000000000000000 ) ) ;
#9228 = DIRECTION ( 'NONE',  ( 0.000000000000000000, 8.191099868251446680E-34, 1.000000000000000000 ) ) ;
#9229 = FACE_OUTER_BOUND ( 'NONE', #8151, .T. ) ;
#9230 = CARTESIAN_POINT ( 'NONE',  ( -6.717514421272238856, 6.717514421272181124, 6.000000000000005329 ) ) ;
#9231 = CARTESIAN_POINT ( 'NONE',  ( 8.922933199037192509, -4.490180821391404287, 14.34886208192142831 ) ) ;
#9232 = CARTESIAN_POINT ( 'NONE',  ( -7.424621202458789426, 7.424621202458724589, 12.00000000000001066 ) ) ;
#9233 = CARTESIAN_POINT ( 'NONE',  ( -13.82664651025767100, 8.841785722321537477, 21.78975485534072476 ) ) ;
#9234 = CARTESIAN_POINT ( 'NONE',  ( -15.89939535829186923, -1.791431617653016062, 47.14285714285714590 ) ) ;
#9235 =( NAMED_UNIT ( * ) PLANE_ANGLE_UNIT ( ) SI_UNIT ( $, .RADIAN. ) );
#9236 = CARTESIAN_POINT ( 'NONE',  ( -13.82664651025767100, 8.841785722321537477, 15.78975485534072121 ) ) ;
#9237 = CARTESIAN_POINT ( 'NONE',  ( -13.55419868402807992, -4.742819248065651472, 28.92857142857143771 ) ) ;
#9238 = CARTESIAN_POINT ( 'NONE',  ( 5.420364854932001819, 15.49051278174644430, 7.071428571428569398 ) ) ;
#9239 = CARTESIAN_POINT ( 'NONE',  ( -5.284464991282755264, 15.10213328493384743, 42.42857142857143060 ) ) ;
#9240 = EDGE_LOOP ( 'NONE', ( #10150, #6633 ) ) ;
#9241 = CARTESIAN_POINT ( 'NONE',  ( -1.727091770866549414, -10.90442828429184630, 13.95000000000002593 ) ) ;
#9242 = DIRECTION ( 'NONE',  ( 0.000000000000000000, -6.338944243255235518E-49, 1.000000000000000000 ) ) ;
#9243 = CARTESIAN_POINT ( 'NONE',  ( -13.54758718765249625, -8.512513224245459753, 40.71428571428571530 ) ) ;
#9244 = DIRECTION ( 'NONE',  ( 0.000000000000000000, 0.000000000000000000, 1.000000000000000000 ) ) ;
#9245 = CARTESIAN_POINT ( 'NONE',  ( 7.340858601237956194, 11.92174236212700045, 9.281673716087846415 ) ) ;
#9246 = CARTESIAN_POINT ( 'NONE',  ( 1.727091770866550968, 10.90442828429187294, 15.44999999999997797 ) ) ;
#9247 = CARTESIAN_POINT ( 'NONE',  ( -5.284464991282755264, 15.10213328493384743, 6.428571428571429713 ) ) ;
#9248 = CARTESIAN_POINT ( 'NONE',  ( -16.29368510291090288, 1.967016585148476215, 45.36118342676930837 ) ) ;
#9249 = PRODUCT_CONTEXT ( 'NONE', #6976, 'mechanical' ) ;
#9250 = CARTESIAN_POINT ( 'NONE',  ( -4.742819248065500481, -13.55419868402813499, 22.07142857142858006 ) ) ;
#9251 = CARTESIAN_POINT ( 'NONE',  ( 7.529642458189280241, -12.22833218042435099, 25.21832628391215181 ) ) ;
#9252 = VERTEX_POINT ( 'NONE', #5175 ) ;
#9253 = CARTESIAN_POINT ( 'NONE',  ( 4.743843029824831525, -13.17239914596749095, 35.42453085894499765 ) ) ;
#9254 = AXIS2_PLACEMENT_3D ( 'NONE', #9597, #7051, #4110 ) ;
#9255 = ORIENTED_EDGE ( 'NONE', *, *, #1061, .F. ) ;
#9256 = FACE_BOUND ( 'NONE', #3279, .T. ) ;
#9257 = CARTESIAN_POINT ( 'NONE',  ( -5.297344310588352201, -15.53355953199867301, 30.06738800180214355 ) ) ;
#9258 = CARTESIAN_POINT ( 'NONE',  ( -156.0000000000000284, 15.99999999999999289, 1.959434878635764737E-15 ) ) ;
#9259 = CARTESIAN_POINT ( 'NONE',  ( -7.458344646081709328, 7.390897758835805575, 18.99886208192142334 ) ) ;
#9260 = CARTESIAN_POINT ( 'NONE',  ( -9.989344678689363377, 9.809645194533960222, 49.99595943037357415 ) ) ;
#9261 = CARTESIAN_POINT ( 'NONE',  ( -4.766900247265192014, -9.355568503977876205, 2.099999999999990763 ) ) ;
#9262 = CARTESIAN_POINT ( 'NONE',  ( 9.814260835641038128, -5.056896391392198709, 18.35113791807858519 ) ) ;
#9263 = CARTESIAN_POINT ( 'NONE',  ( 2.000000000000001776, 1.773042676681366281, 0.000000000000000000 ) ) ;
#9264 = CIRCLE ( 'NONE', #2978, 8.200000000000001066 ) ;
#9265 = VECTOR ( 'NONE', #1939, 1000.000000000000000 ) ;
#9266 = AXIS2_PLACEMENT_3D ( 'NONE', #5377, #6241, #3834 ) ;
#9267 = ORIENTED_EDGE ( 'NONE', *, *, #7221, .F. ) ;
#9268 = CARTESIAN_POINT ( 'NONE',  ( 1.441234910513245149, 13.92619789766829008, 2.853102287516426916 ) ) ;
#9269 = EDGE_CURVE ( 'NONE', #2970, #8205, #1509, .T. ) ;
#9270 = CARTESIAN_POINT ( 'NONE',  ( 4.766900247265192903, 9.355568503977902850, 3.599999999999992095 ) ) ;
#9271 = CARTESIAN_POINT ( 'NONE',  ( -8.512513224245306986, -13.54758718765259218, 28.28571428571428825 ) ) ;
#9272 = LINE ( 'NONE', #6866, #8658 ) ;
#9273 = AXIS2_PLACEMENT_3D ( 'NONE', #6842, #3237, #4891 ) ;
#9274 = MECHANICAL_DESIGN_GEOMETRIC_PRESENTATION_REPRESENTATION (  '', ( #6422 ), #3801 ) ;
#9275 = CARTESIAN_POINT ( 'NONE',  ( -14.28433602490915000, 1.478298951650542481, 13.35310228751641937 ) ) ;
#9276 = CARTESIAN_POINT ( 'NONE',  ( 10.36326688006723984, -1.689666864740212215, 0.2011379180785754783 ) ) ;
#9277 = CARTESIAN_POINT ( 'NONE',  ( 9.873755945037075321, 1.513077731353043243, 9.051137918078573819 ) ) ;
#9278 = CARTESIAN_POINT ( 'NONE',  ( -165.9526703272678958, -1.932542173981024458, 12.85566991495389466 ) ) ;
#9279 = CARTESIAN_POINT ( 'NONE',  ( -15.91362231745475597, -1.665163862720028254, 45.14689771248358596 ) ) ;
#9280 = CARTESIAN_POINT ( 'NONE',  ( 4.742819248065503146, 13.55419868402813677, 49.07142857142859071 ) ) ;
#9281 = CARTESIAN_POINT ( 'NONE',  ( 7.448449071214646722, 11.85413878919601594, 49.28571428571428470 ) ) ;
#9282 = VERTEX_POINT ( 'NONE', #6551 ) ;
#9283 = CARTESIAN_POINT ( 'NONE',  ( 1.967016585148662289, -16.29368510291087091, 5.638816573230711171 ) ) ;
#9284 = EDGE_CURVE ( 'NONE', #1035, #557, #4643, .T. ) ;
#9285 = CARTESIAN_POINT ( 'NONE',  ( 15.44569104238500046, -1.018491042385001544, 0.000000000000000000 ) ) ;
#9286 = CARTESIAN_POINT ( 'NONE',  ( 1.791431617652837316, 15.89939535829188877, 36.85714285714286120 ) ) ;
#9287 = FACE_BOUND ( 'NONE', #2507, .T. ) ;
#9288 = PRODUCT_DEFINITION ( 'UNKNOWN', '', #4927, #9809 ) ;
#9289 = CARTESIAN_POINT ( 'NONE',  ( -88.00000000000002842, 0.000000000000000000, 0.000000000000000000 ) ) ;
#9290 = CARTESIAN_POINT ( 'NONE',  ( 8.464561979789474222, 4.312909747525755400, 3.899999999999959055 ) ) ;
#9291 = CARTESIAN_POINT ( 'NONE',  ( 1.533232399700100945, -9.375578539472067874, 17.79886208192143471 ) ) ;
#9292 = CARTESIAN_POINT ( 'NONE',  ( 2.000000000000001776, 0.8865213383407039016, -1.535500000000022958 ) ) ;
#9293 = CARTESIAN_POINT ( 'NONE',  ( -15.06016580658428694, 5.404401153735006957, 21.57546914105500946 ) ) ;
#9294 = CARTESIAN_POINT ( 'NONE',  ( 1.791431617652837316, 15.89939535829188877, 42.85714285714285410 ) ) ;
#9295 = CARTESIAN_POINT ( 'NONE',  ( -5.164528828830334817, 15.14410076328347543, 22.43261199819786356 ) ) ;
#9296 = CARTESIAN_POINT ( 'NONE',  ( 8.731428362939190890, -13.89598863503036164, 15.21428571428571530 ) ) ;
#9297 = CARTESIAN_POINT ( 'NONE',  ( 3.909482873968459948, 15.52014209590646310, 48.73000000000003951 ) ) ;
#9298 = ORIENTED_EDGE ( 'NONE', *, *, #3626, .F. ) ;
#9299 = PLANE ( 'NONE',  #640 ) ;
#9300 = CARTESIAN_POINT ( 'NONE',  ( 2.000000000000001776, 0.000000000000000000, 0.000000000000000000 ) ) ;
#9301 = CARTESIAN_POINT ( 'NONE',  ( -13.89598863503045933, 8.731428362939027465, 41.78571428571429180 ) ) ;
#9302 = CARTESIAN_POINT ( 'NONE',  ( -9.333916720356675967, -4.809394265263095214, 12.39886208192140948 ) ) ;
#9303 = CARTESIAN_POINT ( 'NONE',  ( -15.89939535829186923, -1.791431617653016062, 5.142857142857143238 ) ) ;
#9304 = CIRCLE ( 'NONE', #2201, 18.00000000000000355 ) ;
#9305 = CARTESIAN_POINT ( 'NONE',  ( -1.567502665446231180, -13.91197093850540334, 21.85714285714286120 ) ) ;
#9306 = EDGE_CURVE ( 'NONE', #6851, #5977, #5288, .T. ) ;
#9307 = CARTESIAN_POINT ( 'NONE',  ( 13.59724543428031573, 4.619798703722006294, 35.93261199819787066 ) ) ;
#9308 = CARTESIAN_POINT ( 'NONE',  ( -1.486127417882243895, 9.383039235653825472, 6.299999999999972289 ) ) ;
#9309 = CARTESIAN_POINT ( 'NONE',  ( 12.22833218042443271, -7.529642458189144349, 46.78167371608785885 ) ) ;
#9310 = ORIENTED_EDGE ( 'NONE', *, *, #3298, .F. ) ;
#9311 = DIRECTION ( 'NONE',  ( -1.000000000000000000, 0.000000000000000000, 0.000000000000000000 ) ) ;
#9312 = CARTESIAN_POINT ( 'NONE',  ( 1.665163862719847732, 15.91362231745477374, 26.85310228751642470 ) ) ;
#9313 = CARTESIAN_POINT ( 'NONE',  ( -15.89939535829186923, -1.791431617653016062, 5.142857142857143238 ) ) ;
#9314 = CARTESIAN_POINT ( 'NONE',  ( 6.751237864895159646, -6.683790977649233689, 8.498862081921462419 ) ) ;
#9315 = CARTESIAN_POINT ( 'NONE',  ( -8.404922754268618235, -13.61519076058357491, 24.28167371608785530 ) ) ;
#9316 = DIRECTION ( 'NONE',  ( 0.000000000000000000, -1.224646799147353454E-16, 1.000000000000000000 ) ) ;
#9317 = CARTESIAN_POINT ( 'NONE',  ( 10.91227292449344155, 1.677562661911773390, 15.05113791807855961 ) ) ;
#9318 = DIRECTION ( 'NONE',  ( 1.000000000000000000, 0.000000000000000000, 0.000000000000000000 ) ) ;
#9319 = CARTESIAN_POINT ( 'NONE',  ( 4.865839792409144771, 13.51115193377589740, 35.07546914105501656 ) ) ;
#9320 = SURFACE_STYLE_USAGE ( .BOTH. , #1410 ) ;
#9321 = AXIS2_PLACEMENT_3D ( 'NONE', #4044, #4192, #9679 ) ;
#9322 = EDGE_LOOP ( 'NONE', ( #9223, #9515, #3558, #1602, #6397 ) ) ;
#9323 = CARTESIAN_POINT ( 'NONE',  ( 13.89774397934249706, 1.693770420379375308, 4.138816573230708507 ) ) ;
#9324 = DIRECTION ( 'NONE',  ( 0.000000000000000000, -6.338944243255235518E-49, 1.000000000000000000 ) ) ;
#9325 = DIRECTION ( 'NONE',  ( -6.162975822039151993E-33, 0.8660254037844393737, 0.4999999999999987788 ) ) ;
#9326 = CARTESIAN_POINT ( 'NONE',  ( 1.737328882695370558, -14.25515036105620581, 29.63881657323071295 ) ) ;
#9327 = CARTESIAN_POINT ( 'NONE',  ( -1.439022436064386845, 9.390499931835535108, 14.30113791807856316 ) ) ;
#9328 = CARTESIAN_POINT ( 'NONE',  ( 8.877401133907127928, -4.579542530753017537, 3.351137918078579858 ) ) ;
#9329 = CARTESIAN_POINT ( 'NONE',  ( 2.000000000000001776, 0.000000000000000000, 0.000000000000000000 ) ) ;
#9330 = CARTESIAN_POINT ( 'NONE',  ( -7.639999817571787588, 12.15899005565156266, 48.21428571428570820 ) ) ;
#9331 = CARTESIAN_POINT ( 'NONE',  ( 8.784089738577305795, 11.01490013464600892, 49.39149694378009769 ) ) ;
#9332 = EDGE_LOOP ( 'NONE', ( #5521, #2052, #6534, #1798, #8654, #4033 ) ) ;
#9333 = CARTESIAN_POINT ( 'NONE',  ( 11.51250119794888249, 11.69682198916847682, 9.495959430373563492 ) ) ;
#9334 = FACE_OUTER_BOUND ( 'NONE', #7375, .T. ) ;
#9335 = ADVANCED_FACE ( 'NONE', ( #9163, #1966 ), #2070, .T. ) ;
#9336 = CARTESIAN_POINT ( 'NONE',  ( -1.791431617652833763, -15.89939535829188877, 33.85714285714285410 ) ) ;
#9337 = FACE_OUTER_BOUND ( 'NONE', #8020, .T. ) ;
#9338 = DIRECTION ( 'NONE',  ( 0.000000000000000000, 8.191099868251448390E-34, 1.000000000000000000 ) ) ;
#9339 = CARTESIAN_POINT ( 'NONE',  ( 10.37072757624895836, -1.642561882922355831, 1.200000000000034373 ) ) ;
#9340 = CARTESIAN_POINT ( 'NONE',  ( 4.312909747525650594, 8.464561979789532842, 3.599999999999992095 ) ) ;
#9341 = CARTESIAN_POINT ( 'NONE',  ( 6.751237864895159646, -6.683790977649233689, 17.49886208192142689 ) ) ;
#9342 = CYLINDRICAL_SURFACE ( 'NONE', #4464, 16.00000000000000000 ) ;
#9343 =( NAMED_UNIT ( * ) PLANE_ANGLE_UNIT ( ) SI_UNIT ( $, .RADIAN. ) );
#9344 = CARTESIAN_POINT ( 'NONE',  ( -8.620103694221995738, -13.47998361472161299, 14.28975485534072298 ) ) ;
#9345 = CARTESIAN_POINT ( 'NONE',  ( 15.49051278174638036, 5.420364854932175014, 13.92857142857143238 ) ) ;
#9346 = LINE ( 'NONE', #3962, #7932 ) ;
#9347 = CARTESIAN_POINT ( 'NONE',  ( -9.355568503977838901, -4.766900247265279944, 11.39999999999996660 ) ) ;
#9348 = ORIENTED_EDGE ( 'NONE', *, *, #3669, .F. ) ;
#9349 = EDGE_CURVE ( 'NONE', #5718, #6987, #181, .T. ) ;
#9350 = LINE ( 'NONE', #9968, #1012 ) ;
#9351 = CARTESIAN_POINT ( 'NONE',  ( 9.333916720356675967, 4.809394265263126300, 7.898862081921404155 ) ) ;
#9352 = CARTESIAN_POINT ( 'NONE',  ( -8.731428362939189114, 13.89598863503036341, 6.214285714285717965 ) ) ;
#9353 = CARTESIAN_POINT ( 'NONE',  ( -15.91362231745475597, -1.665163862720028254, 45.14689771248358596 ) ) ;
#9354 = CONTEXT_DEPENDENT_SHAPE_REPRESENTATION ( #7315, #2691 ) ;
#9355 = CARTESIAN_POINT ( 'NONE',  ( 7.448449071214646722, 11.85413878919601594, 19.28571428571428825 ) ) ;
#9356 = CARTESIAN_POINT ( 'NONE',  ( -10.24623928997352351, -10.06191849875416899, 38.50404056962644006 ) ) ;
#9357 = CARTESIAN_POINT ( 'NONE',  ( 4.534861676072321046, -8.900167166472098046, 10.65000000000001101 ) ) ;
#9358 = ORIENTED_EDGE ( 'NONE', *, *, #10144, .F. ) ;
#9359 = CARTESIAN_POINT ( 'NONE',  ( 11.78653521626494793, 7.556039541191463371, 39.71024514465927524 ) ) ;
#9360 = VERTEX_POINT ( 'NONE', #9734 ) ;
#9361 = CARTESIAN_POINT ( 'NONE',  ( 15.14410076328353227, -5.164528828830166063, 16.56738800180213289 ) ) ;
#9362 = CARTESIAN_POINT ( 'NONE',  ( -5.284464991282755264, 15.10213328493384743, 6.428571428571429713 ) ) ;
#9363 = CARTESIAN_POINT ( 'NONE',  ( 4.270415729527831772, 8.486213763410697553, 7.598862081921438971 ) ) ;
#9364 = CARTESIAN_POINT ( 'NONE',  ( -15.14410076328353227, 5.164528828830164287, 19.56738800180213644 ) ) ;
#9365 = CARTESIAN_POINT ( 'NONE',  ( -1.727091770866549414, -10.90442828429184630, 1.949999999999996181 ) ) ;
#9366 = CARTESIAN_POINT ( 'NONE',  ( -1.776620879821455556, -10.89658364409025637, 15.95113791807857595 ) ) ;
#9367 = DIRECTION ( 'NONE',  ( 0.000000000000000000, -1.000000000000000000, 0.000000000000000000 ) ) ;
#9368 = CARTESIAN_POINT ( 'NONE',  ( 10.24623928997352884, 10.06191849875416899, 41.50404056962644006 ) ) ;
#9369 = CIRCLE ( 'NONE', #3911, 15.00000000000000000 ) ;
#9370 =( NAMED_UNIT ( * ) PLANE_ANGLE_UNIT ( ) SI_UNIT ( $, .RADIAN. ) );
#9371 = CARTESIAN_POINT ( 'NONE',  ( -10.06191849875405531, -10.24623928997363542, 6.495959430373559051 ) ) ;
#9372 = CARTESIAN_POINT ( 'NONE',  ( 9.837026868206070418, -5.012215536711392083, 7.350000000000000533 ) ) ;
#9373 = EDGE_CURVE ( 'NONE', #8713, #2655, #318, .T. ) ;
#9374 = LINE ( 'NONE', #2386, #2866 ) ;
#9375 = PRESENTATION_LAYER_ASSIGNMENT (  '', '', ( #116 ) ) ;
#9376 = CARTESIAN_POINT ( 'NONE',  ( 7.842167650704563897, 7.771249796623202144, 8.751137918078539357 ) ) ;
#9377 = CARTESIAN_POINT ( 'NONE',  ( 7.098671581784200768, 7.027753727702831021, 5.751137918078548239 ) ) ;
#9378 = CARTESIAN_POINT ( 'NONE',  ( -162.8500000000000512, -5.808233196467851957E-15, 13.00000000000000178 ) ) ;
#9379 = CARTESIAN_POINT ( 'NONE',  ( -15.06016580658428694, 5.404401153735006957, 45.57546914105501656 ) ) ;
#9380 = CARTESIAN_POINT ( 'NONE',  ( -4.865839792409144771, -13.51115193377589740, 8.075469141055007682 ) ) ;
#9381 = CARTESIAN_POINT ( 'NONE',  ( 9.899494936611610285, 9.899494936611718643, 49.50000000000000711 ) ) ;
#9382 = ORIENTED_EDGE ( 'NONE', *, *, #9119, .F. ) ;
#9383 = CARTESIAN_POINT ( 'NONE',  ( 8.404922754268618235, 13.61519076058357491, 15.28167371608785174 ) ) ;
#9384 = CARTESIAN_POINT ( 'NONE',  ( -88.00000000000002842, 1.592040838891559095E-15, -13.00000000000000000 ) ) ;
#9385 = CARTESIAN_POINT ( 'NONE',  ( -1.791431617652833763, -15.89939535829188877, 39.85714285714286120 ) ) ;
#9386 = MECHANICAL_DESIGN_GEOMETRIC_PRESENTATION_REPRESENTATION (  '', ( #4756 ), #1279 ) ;
#9387 = CARTESIAN_POINT ( 'NONE',  ( -58.00000000000002132, 1.249000902703378268E-16, 18.00000000000002132 ) ) ;
#9388 = CARTESIAN_POINT ( 'NONE',  ( 0.000000000000000000, -1.773042676681352292, -1.110223024625156540E-13 ) ) ;
#9389 = CARTESIAN_POINT ( 'NONE',  ( 6.683790977649321619, -6.751237864895077045, 0.5011379180785839882 ) ) ;
#9390 = CARTESIAN_POINT ( 'NONE',  ( 7.063212654743467489, 7.063212654743557195, 0.7499999999999762412 ) ) ;
#9391 = LINE ( 'NONE', #9292, #8928 ) ;
#9392 = CARTESIAN_POINT ( 'NONE',  ( -9.383039235653820143, 1.486127417882155299, 2.700000000000035705 ) ) ;
#9393 =( LENGTH_UNIT ( ) NAMED_UNIT ( * ) SI_UNIT ( .MILLI., .METRE. ) );
#9394 = PRODUCT_DEFINITION_FORMATION_WITH_SPECIFIED_SOURCE ( 'ANY', '', #1874, .NOT_KNOWN. ) ;
#9395 = CARTESIAN_POINT ( 'NONE',  ( 15.53355953199861794, 5.297344310588528060, 17.93261199819786711 ) ) ;
#9396 = VERTEX_POINT ( 'NONE', #5066 ) ;
#9397 = CARTESIAN_POINT ( 'NONE',  ( -5.284464991282755264, 15.10213328493384743, 24.42857142857143060 ) ) ;
#9398 = DIRECTION ( 'NONE',  ( 0.000000000000000000, 8.191099868251448390E-34, 1.000000000000000000 ) ) ;
#9399 = LINE ( 'NONE', #4017, #1983 ) ;
#9400 = ADVANCED_FACE ( 'NONE', ( #8959 ), #8436, .F. ) ;
#9401 = CARTESIAN_POINT ( 'NONE',  ( -0.3453160816774686892, 15.99627321608801367, 48.73000000000002530 ) ) ;
#9402 = CARTESIAN_POINT ( 'NONE',  ( 10.89658364409024749, 1.776620879821585897, 5.048862081921459577 ) ) ;
#9403 = CARTESIAN_POINT ( 'NONE',  ( -11.31370849898482156, 11.31370849898469544, 0.000000000000000000 ) ) ;
#9404 = ITEM_DEFINED_TRANSFORMATION ( 'NONE', 'NONE', #1626,  #3995 ) ;
#9405 = CARTESIAN_POINT ( 'NONE',  ( 13.21436662431716869, -4.623906867372263640, 44.57142857142857650 ) ) ;
#9406 = CARTESIAN_POINT ( 'NONE',  ( 14.25515036105622535, -1.737328882695210241, 30.36118342676929771 ) ) ;
#9407 = CARTESIAN_POINT ( 'NONE',  ( -8.464561979789474222, -4.312909747525728754, 11.39999999999996660 ) ) ;
#9408 = CARTESIAN_POINT ( 'NONE',  ( -1.727091770866549414, -10.90442828429184630, 16.94999999999998863 ) ) ;
#9409 = VERTEX_POINT ( 'NONE', #6695 ) ;
#9410 = CARTESIAN_POINT ( 'NONE',  ( -13.25633410266679313, 4.503970704919840529, 43.56738800180213644 ) ) ;
#9411 = CYLINDRICAL_SURFACE ( 'NONE', #2268, 2.149999999999985256 ) ;
#9412 = CARTESIAN_POINT ( 'NONE',  ( -8.841785722321695573, 13.82664651025757152, 20.21024514465928235 ) ) ;
#9413 = CARTESIAN_POINT ( 'NONE',  ( -11.60466159355861748, -11.60466159355874893, 10.50000000000000355 ) ) ;
#9414 = CARTESIAN_POINT ( 'NONE',  ( 4.270415729527831772, 8.486213763410688671, 13.59886208192144430 ) ) ;
#9415 = PRODUCT_DEFINITION ( 'UNKNOWN', '', #2611, #3494 ) ;
#9416 = CARTESIAN_POINT ( 'NONE',  ( 15.88516839912898071, 1.917699372586004092, 22.13881657323070939 ) ) ;
#9417 = CARTESIAN_POINT ( 'NONE',  ( 56.99999999999997158, 9.797174393178825657E-16, -8.000000000000000000 ) ) ;
#9418 = CARTESIAN_POINT ( 'NONE',  ( 4.766900247265192903, 9.355568503977911732, 9.599999999999997868 ) ) ;
#9419 = CARTESIAN_POINT ( 'NONE',  ( 61.99999999999997158, 0.000000000000000000, 8.000000000000000000 ) ) ;
#9420 =( LENGTH_UNIT ( ) NAMED_UNIT ( * ) SI_UNIT ( .MILLI., .METRE. ) );
#9421 = AXIS2_PLACEMENT_3D ( 'NONE', #1586, #8711, #3124 ) ;
#9422 = ORIENTED_EDGE ( 'NONE', *, *, #4530, .T. ) ;
#9423 = CARTESIAN_POINT ( 'NONE',  ( -1.967016585148659846, 16.29368510291087091, 50.63881657323071295 ) ) ;
#9424 = CARTESIAN_POINT ( 'NONE',  ( -5.110041130070070992, -16.97680807127747826, -1.270000000000007123 ) ) ;
#9425 = FACE_OUTER_BOUND ( 'NONE', #6823, .T. ) ;
#9426 = CARTESIAN_POINT ( 'NONE',  ( -13.51115193377584589, -4.865839792409295761, 24.92453085894499765 ) ) ;
#9427 = CARTESIAN_POINT ( 'NONE',  ( 1.776620879821457333, 10.89658364409028124, 2.451137918078564848 ) ) ;
#9429 = CIRCLE ( 'NONE', #7602, 18.00000000000000355 ) ;
#9428 = CARTESIAN_POINT ( 'NONE',  ( -4.490180821391513533, 8.922933199037158758, 17.15113791807853616 ) ) ;
#9430 = AXIS2_PLACEMENT_3D ( 'NONE', #805, #2502, #4932 ) ;
#9431 = CARTESIAN_POINT ( 'NONE',  ( -165.5557670730357529, -2.081659637464541301, 12.83228186348094901 ) ) ;
#9432 = CARTESIAN_POINT ( 'NONE',  ( 13.92619789766827587, 1.441234910513398582, 6.146897712483580634 ) ) ;
#9433 = CARTESIAN_POINT ( 'NONE',  ( 4.865839792409144771, 13.51115193377589740, 5.075469141055008571 ) ) ;
#9434 = ORIENTED_EDGE ( 'NONE', *, *, #3066, .T. ) ;
#9435 = EDGE_CURVE ( 'NONE', #7562, #9409, #9787, .T. ) ;
#9436 = CARTESIAN_POINT ( 'NONE',  ( 5.297344310588354865, 15.53355953199867301, 9.067388001802141773 ) ) ;
#9437 = STYLED_ITEM ( 'NONE', ( #6375 ), #7077 ) ;
#9438 = DIRECTION ( 'NONE',  ( 0.000000000000000000, 8.191099868251446680E-34, 1.000000000000000000 ) ) ;
#9439 = VECTOR ( 'NONE', #525, 1000.000000000000000 ) ;
#9440 = ADVANCED_FACE ( 'NONE', ( #8215, #1144 ), #4290, .F. ) ;
#9441 = CARTESIAN_POINT ( 'NONE',  ( 5.284464991282756152, -15.10213328493384743, 45.42857142857143060 ) ) ;
#9442 = CARTESIAN_POINT ( 'NONE',  ( 5.110041130070070992, -16.97680807127747826, 0.000000000000000000 ) ) ;
#9443 = CARTESIAN_POINT ( 'NONE',  ( -170.0000000000000284, -11.00000000000000533, 0.000000000000000000 ) ) ;
#9444 = APPLICATION_CONTEXT ( 'automotive_design' ) ;
#9445 = CARTESIAN_POINT ( 'NONE',  ( 1.612135949262739398, 9.858066664633913234, -0.5488620819214271584 ) ) ;
#9446 = CARTESIAN_POINT ( 'NONE',  ( -1.513077731352923339, -9.873755945037078874, 14.94886208192145105 ) ) ;
#9447 = DIRECTION ( 'NONE',  ( 0.2882273949230682586, -0.9575619921529162637, -1.755378125195845577E-33 ) ) ;
#9448 = CARTESIAN_POINT ( 'NONE',  ( -5.543385399275643444, -15.44746603149420494, 32.07546914105502367 ) ) ;
#9449 = CARTESIAN_POINT ( 'NONE',  ( -4.534861676072319270, 8.900167166472122915, 3.149999999999958611 ) ) ;
#9450 = MECHANICAL_DESIGN_GEOMETRIC_PRESENTATION_REPRESENTATION (  '', ( #3653 ), #8786 ) ;
#9451 = CARTESIAN_POINT ( 'NONE',  ( -8.620103694221995738, -13.47998361472161299, 38.28975485534072476 ) ) ;
#9452 = CARTESIAN_POINT ( 'NONE',  ( -8.731428362939189114, 13.89598863503036341, 18.21428571428571885 ) ) ;
#9453 = CARTESIAN_POINT ( 'NONE',  ( 0.000000000000000000, 0.8865213383407039016, -1.535500000000022958 ) ) ;
#9454 = CARTESIAN_POINT ( 'NONE',  ( -5.284464991282755264, 15.10213328493384743, 0.4285714285714309346 ) ) ;
#9455 = CLOSED_SHELL ( 'NONE', ( #1076, #4264, #3959, #7548 ) ) ;
#9456 = PRESENTATION_STYLE_ASSIGNMENT (( #8089 ) ) ;
#9457 = CIRCLE ( 'NONE', #3170, 1.000000000000000000 ) ;
#9458 = ADVANCED_BREP_SHAPE_REPRESENTATION ( '', ( #206, #3995 ), #6704 ) ;
#9459 = CARTESIAN_POINT ( 'NONE',  ( 7.771249796623105333, 7.842167650704654491, 13.74886208192144643 ) ) ;
#9460 = CARTESIAN_POINT ( 'NONE',  ( 15.49051278174638036, 5.420364854932175014, 7.928571428571430602 ) ) ;
#9461 = CARTESIAN_POINT ( 'NONE',  ( 1.791431617652837316, 15.89939535829188877, 18.85714285714285765 ) ) ;
#9462 = CARTESIAN_POINT ( 'NONE',  ( 4.623906867372411078, -13.21436662431711717, 33.42857142857143060 ) ) ;
#9463 = ADVANCED_FACE ( 'NONE', ( #2734 ), #7436, .F. ) ;
#9464 = CARTESIAN_POINT ( 'NONE',  ( -13.59724543428031573, -4.619798703722008959, 32.93261199819787777 ) ) ;
#9465 = CARTESIAN_POINT ( 'NONE',  ( 4.534861676072321046, -8.900167166472098046, 13.65000000000003411 ) ) ;
#9466 = CARTESIAN_POINT ( 'NONE',  ( 1.677562661911645714, 10.91227292449347175, 1.448862081921441947 ) ) ;
#9467 = CARTESIAN_POINT ( 'NONE',  ( 7.639999817571789364, -12.15899005565156266, 9.214285714285717077 ) ) ;
#9468 = ORIENTED_EDGE ( 'NONE', *, *, #3511, .T. ) ;
#9469 = DIRECTION ( 'NONE',  ( -0.7063021515967564667, -0.7063021515967625730, -0.04769215134145720486 ) ) ;
#9470 = CARTESIAN_POINT ( 'NONE',  ( -1.967016585148659846, 16.29368510291087091, 32.63881657323070584 ) ) ;
#9471 = EDGE_CURVE ( 'NONE', #5655, #1237, #7712, .T. ) ;
#9472 = CARTESIAN_POINT ( 'NONE',  ( -5.420364854931998266, -15.49051278174643898, 10.07142857142856940 ) ) ;
#9473 = CIRCLE ( 'NONE', #3532, 1.610000000000000098 ) ;
#9474 = CARTESIAN_POINT ( 'NONE',  ( -13.47998361472151174, -8.620103694222146729, 30.71024514465928235 ) ) ;
#9475 = DIRECTION ( 'NONE',  ( 1.387778780781445676E-16, -1.000000000000000000, 0.000000000000000000 ) ) ;
#9476 = CARTESIAN_POINT ( 'NONE',  ( -4.766900247265192014, -9.355568503977876205, 5.099999999999993427 ) ) ;
#9477 = CARTESIAN_POINT ( 'NONE',  ( -108.0000000000000426, -15.99999999999999289, 0.000000000000000000 ) ) ;
#9478 = ORIENTED_EDGE ( 'NONE', *, *, #6620, .F. ) ;
#9479 = EDGE_CURVE ( 'NONE', #2833, #2841, #1294, .T. ) ;
#9480 = CARTESIAN_POINT ( 'NONE',  ( 1.441234910513245149, 13.92619789766829008, 14.85310228751642470 ) ) ;
#9481 = CARTESIAN_POINT ( 'NONE',  ( -7.424621202458789426, 7.424621202458724589, 12.00000000000001066 ) ) ;
#9482 = CARTESIAN_POINT ( 'NONE',  ( 11.60466159355862104, 11.60466159355875071, 13.50000000000000178 ) ) ;
#9483 = DIRECTION ( 'NONE',  ( 0.000000000000000000, 6.938893903907221444E-18, 1.000000000000000000 ) ) ;
#9484 = CARTESIAN_POINT ( 'NONE',  ( -4.809394265263009061, -9.333916720356716823, 7.101137918078564759 ) ) ;
#9485 = CARTESIAN_POINT ( 'NONE',  ( 4.809394265263009061, 9.333916720356739916, -0.3988620819214416247 ) ) ;
#9486 = CARTESIAN_POINT ( 'NONE',  ( -88.00000000000002842, 0.000000000000000000, 0.000000000000000000 ) ) ;
#9487 = CARTESIAN_POINT ( 'NONE',  ( 9.809645194534072132, -9.989344678689256796, 1.004040569626440726 ) ) ;
#9488 = ORIENTED_EDGE ( 'NONE', *, *, #9010, .F. ) ;
#9489 = CARTESIAN_POINT ( 'NONE',  ( 13.96533075980324234, -8.621071003556521006, 16.78167371608784819 ) ) ;
#9490 = CARTESIAN_POINT ( 'NONE',  ( -88.00000000000002842, 0.000000000000000000, 0.000000000000000000 ) ) ;
#9491 = CARTESIAN_POINT ( 'NONE',  ( -15.10213328493390961, 5.284464991282586510, 47.57142857142857650 ) ) ;
#9492 = FACE_OUTER_BOUND ( 'NONE', #940, .T. ) ;
#9493 = DIRECTION ( 'NONE',  ( -1.000000000000000000, -0.000000000000000000, -0.000000000000000000 ) ) ;
#9494 = CARTESIAN_POINT ( 'NONE',  ( -4.312909747525649706, -8.464561979789507973, 17.10000000000000497 ) ) ;
#9495 = CARTESIAN_POINT ( 'NONE',  ( 4.312909747525650594, 8.464561979789532842, 3.599999999999992095 ) ) ;
#9496 = LINE ( 'NONE', #710, #688 ) ;
#9497 = CARTESIAN_POINT ( 'NONE',  ( 5.543385399275644332, 15.44746603149420494, 23.07546914105501301 ) ) ;
#9498 = CARTESIAN_POINT ( 'NONE',  ( 0.000000000000000000, 0.000000000000000000, 68.00000000000000000 ) ) ;
#9499 = CARTESIAN_POINT ( 'NONE',  ( 8.620103694221997515, 13.47998361472160767, 35.28975485534072476 ) ) ;
#9500 = ORIENTED_EDGE ( 'NONE', *, *, #7221, .T. ) ;
#9501 = CARTESIAN_POINT ( 'NONE',  ( 8.731428362939190890, -13.89598863503036164, 21.21428571428571885 ) ) ;
#9502 = CARTESIAN_POINT ( 'NONE',  ( -108.0000000000000426, 0.000000000000000000, 0.000000000000000000 ) ) ;
#9503 = EDGE_LOOP ( 'NONE', ( #6207, #5388, #8318, #2054 ) ) ;
#9504 = CARTESIAN_POINT ( 'NONE',  ( -5.420364854931999155, -15.49051278174644253, 4.071428571428569398 ) ) ;
#9505 = ADVANCED_FACE ( 'NONE', ( #4660 ), #8533, .F. ) ;
#9506 = PRESENTATION_STYLE_ASSIGNMENT (( #6324 ) ) ;
#9507 = CARTESIAN_POINT ( 'NONE',  ( 9.390499931835536884, -1.439022436064273158, 2.198862081921450606 ) ) ;
#9508 = CARTESIAN_POINT ( 'NONE',  ( 7.771249796623105333, 7.842167650704658932, 7.748862081921418010 ) ) ;
#9509 = CARTESIAN_POINT ( 'NONE',  ( 8.621071003556677326, -13.96533075980314287, 1.218326283912148922 ) ) ;
#9510 = CARTESIAN_POINT ( 'NONE',  ( 15.89939535829187278, 1.791431617653015174, 20.14285714285714235 ) ) ;
#9511 = CARTESIAN_POINT ( 'NONE',  ( -4.623906867372410190, 13.21436662431711895, 36.42857142857143060 ) ) ;
#9512 = CARTESIAN_POINT ( 'NONE',  ( 13.59724543428031573, 4.619798703722006294, 29.93261199819786356 ) ) ;
#9513 = CARTESIAN_POINT ( 'NONE',  ( -6.717514421272238856, 6.717514421272180236, 9.000000000000007105 ) ) ;
#9514 = CARTESIAN_POINT ( 'NONE',  ( 1.689666864740335894, -10.36326688006721497, 2.798862081921426714 ) ) ;
#9515 = ORIENTED_EDGE ( 'NONE', *, *, #8953, .F. ) ;
#9516 = CARTESIAN_POINT ( 'NONE',  ( 13.91197093850538380, 1.567502665446386390, 2.142857142857140573 ) ) ;
#9517 = EDGE_LOOP ( 'NONE', ( #5644, #715, #7532, #6035 ) ) ;
#9518 = DIRECTION ( 'NONE',  ( 0.000000000000000000, -1.000000000000000000, 9.714451465470119729E-16 ) ) ;
#9519 = CARTESIAN_POINT ( 'NONE',  ( -16.30827793483735988, 1.837501619626141558, 17.35714285714286120 ) ) ;
#9520 = CARTESIAN_POINT ( 'NONE',  ( -11.51250119794888072, -11.69682198916848037, 18.49595943037356705 ) ) ;
#9521 = CARTESIAN_POINT ( 'NONE',  ( 1.727091770866550968, 10.90442828429187294, 3.450000000000006839 ) ) ;
#9522 = CARTESIAN_POINT ( 'NONE',  ( 10.37072757624895836, -1.642561882922355831, 1.200000000000034373 ) ) ;
#9523 = CARTESIAN_POINT ( 'NONE',  ( 13.21436662431716869, -4.623906867372263640, 2.571428571428571619 ) ) ;
#9524 = CARTESIAN_POINT ( 'NONE',  ( 5.284464991282756152, -15.10213328493384743, 33.42857142857143060 ) ) ;
#9525 = ORIENTED_EDGE ( 'NONE', *, *, #8842, .F. ) ;
#9526 = CARTESIAN_POINT ( 'NONE',  ( 13.51115193377584589, 4.865839792409294873, 9.924530858944988765 ) ) ;
#9527 = CARTESIAN_POINT ( 'NONE',  ( -10.37072757624895836, 1.642561882922380923, 17.69999999999999218 ) ) ;
#9528 = CARTESIAN_POINT ( 'NONE',  ( 15.10213328493390783, -5.284464991282587398, 14.57142857142856940 ) ) ;
#9529 = CARTESIAN_POINT ( 'NONE',  ( -165.7311118698760026, 1.483131377360883185, 12.91518709242523855 ) ) ;
#9530 = CARTESIAN_POINT ( 'NONE',  ( -13.89774397934249706, -1.693770420379375974, 25.13881657323070939 ) ) ;
#9531 = CARTESIAN_POINT ( 'NONE',  ( -4.809394265263009061, -9.333916720356718599, 1.101137918078559208 ) ) ;
#9532 = CARTESIAN_POINT ( 'NONE',  ( 4.355403765523470305, 8.442910196168369907, 14.60113791807856920 ) ) ;
#9533 = DIRECTION ( 'NONE',  ( -1.000000000000000000, -0.000000000000000000, -0.000000000000000000 ) ) ;
#9534 = CARTESIAN_POINT ( 'NONE',  ( 7.556039541191335474, 11.78653521626503320, -0.7102451446592792372 ) ) ;
#9535 = CARTESIAN_POINT ( 'NONE',  ( 13.17239914596754424, -4.743843029824685864, 6.575469141055007682 ) ) ;
#9537 = CARTESIAN_POINT ( 'NONE',  ( -31.74999999999994316, 0.000000000000000000, 0.000000000000000000 ) ) ;
#9536 = AXIS2_PLACEMENT_3D ( 'NONE', #3410, #9827, #6545 ) ;
#9538 = CARTESIAN_POINT ( 'NONE',  ( 5.420364854932001819, 15.49051278174644430, 49.07142857142859071 ) ) ;
#9539 = CARTESIAN_POINT ( 'NONE',  ( -165.1102640658071437, -1.649921999561606567, 12.89487329916352465 ) ) ;
#9540 = DIRECTION ( 'NONE',  ( -4.755747939841215952E-17, 1.000000000000000000, 0.000000000000000000 ) ) ;
#9541 = CARTESIAN_POINT ( 'NONE',  ( -1.439022436064386845, 9.390499931835535108, -0.6988620819214501623 ) ) ;
#9542 = CARTESIAN_POINT ( 'NONE',  ( 4.312909747525650594, 8.464561979789541724, 9.599999999999997868 ) ) ;
#9543 = CARTESIAN_POINT ( 'NONE',  ( -167.1360087209127130, 0.2822104782917173038, 12.99766528766663853 ) ) ;
#9544 = CARTESIAN_POINT ( 'NONE',  ( -11.69682198916834892, -11.51250119794901394, 26.50404056962643651 ) ) ;
#9545 = CARTESIAN_POINT ( 'NONE',  ( 6.717514421272239744, -6.717514421272154479, 1.500000000000001332 ) ) ;
#9546 = CARTESIAN_POINT ( 'NONE',  ( -16.29368510291090288, 1.967016585148476215, 33.36118342676929416 ) ) ;
#9547 = ORIENTED_EDGE ( 'NONE', *, *, #1622, .F. ) ;
#9548 =( GEOMETRIC_REPRESENTATION_CONTEXT ( 3 ) GLOBAL_UNCERTAINTY_ASSIGNED_CONTEXT ( ( #6574 ) ) GLOBAL_UNIT_ASSIGNED_CONTEXT ( ( #6809, #5120, #8273 ) ) REPRESENTATION_CONTEXT ( 'NONE', 'WORKASPACE' ) );
#9549 = CARTESIAN_POINT ( 'NONE',  ( -8.731428362939189114, 13.89598863503036341, 36.21428571428573662 ) ) ;
#9550 = CARTESIAN_POINT ( 'NONE',  ( 1.259487257818240558, 14.39292736161286079, 2.773985284965513663E-17 ) ) ;
#9551 = ORIENTED_EDGE ( 'NONE', *, *, #1818, .F. ) ;
#9552 = CARTESIAN_POINT ( 'NONE',  ( -8.731428362939189114, 13.89598863503036341, 0.2142857142857168273 ) ) ;
#9553 = FACE_OUTER_BOUND ( 'NONE', #7753, .T. ) ;
#9554 = CARTESIAN_POINT ( 'NONE',  ( 5.056896391392317724, -9.814260835640977731, 14.64886208192141659 ) ) ;
#9555 = CARTESIAN_POINT ( 'NONE',  ( 10.89658364409024749, 1.776620879821585897, 2.048862081921423162 ) ) ;
#9556 = CARTESIAN_POINT ( 'NONE',  ( 10.89658364409024749, 1.776620879821587229, 14.04886208192143471 ) ) ;
#9557 = CARTESIAN_POINT ( 'NONE',  ( 1.693770420379222319, 13.89774397934251837, 46.86118342676930126 ) ) ;
#9558 = CARTESIAN_POINT ( 'NONE',  ( -11.60466159355861926, -11.60466159355875249, 16.50000000000000000 ) ) ;
#9559 = CARTESIAN_POINT ( 'NONE',  ( -11.85413878919593422, -7.448449071214776396, 40.71428571428571530 ) ) ;
#9560 = CARTESIAN_POINT ( 'NONE',  ( -1.478298951650703019, 14.28433602490913579, 40.64689771248358596 ) ) ;
#9561 = CARTESIAN_POINT ( 'NONE',  ( -1.607813917173034124, 14.26974319298267524, 12.64285714285714235 ) ) ;
#9562 = FACE_OUTER_BOUND ( 'NONE', #4573, .T. ) ;
#9563 = CARTESIAN_POINT ( 'NONE',  ( 1.727091770866550968, 10.90442828429187294, 15.44999999999997797 ) ) ;
#9564 = ORIENTED_EDGE ( 'NONE', *, *, #2433, .F. ) ;
#9565 = CARTESIAN_POINT ( 'NONE',  ( -9.899494936611716867, 9.899494936611610285, 5.999999999999998224 ) ) ;
#9566 = ORIENTED_EDGE ( 'NONE', *, *, #8953, .T. ) ;
#9567 = DIRECTION ( 'NONE',  ( -0.7071067811865519026, 0.7071067811865432429, -6.110863319087399810E-17 ) ) ;
#9568 = CARTESIAN_POINT ( 'NONE',  ( -16.30827793483735988, 1.837501619626141558, 11.35714285714285765 ) ) ;
#9569 = CARTESIAN_POINT ( 'NONE',  ( -13.96533075980324234, 8.621071003556515677, 43.78167371608784464 ) ) ;
#9570 = CARTESIAN_POINT ( 'NONE',  ( -10.37072757624895836, 1.642561882922380034, 11.69999999999998863 ) ) ;
#9571 = CARTESIAN_POINT ( 'NONE',  ( 1.727091770866550968, 10.90442828429187294, 0.4499999999999856337 ) ) ;
#9572 = CARTESIAN_POINT ( 'NONE',  ( -9.899494936611716867, 9.899494936611610285, 0.000000000000000000 ) ) ;
#9573 = PRESENTATION_STYLE_ASSIGNMENT (( #891 ) ) ;
#9574 = ORIENTED_EDGE ( 'NONE', *, *, #1343, .T. ) ;
#9575 = CARTESIAN_POINT ( 'NONE',  ( -13.89774397934249706, -1.693770420379375974, 19.13881657323070584 ) ) ;
#9576 = CARTESIAN_POINT ( 'NONE',  ( -7.806708723663831506, -7.806708723663903449, 14.25000000000001421 ) ) ;
#9577 = CARTESIAN_POINT ( 'NONE',  ( -166.6500000000000341, -1.532656754117495520E-15, 13.00000000000000355 ) ) ;
#9578 = CARTESIAN_POINT ( 'NONE',  ( -13.25633410266679313, 4.503970704919840529, 43.56738800180213644 ) ) ;
#9579 = CARTESIAN_POINT ( 'NONE',  ( 4.809394265263009061, 9.333916720356739916, 5.601137918078562983 ) ) ;
#9580 = CARTESIAN_POINT ( 'NONE',  ( -8.486213763410637156, -4.270415729527911708, 10.40113791807857524 ) ) ;
#9581 = CARTESIAN_POINT ( 'NONE',  ( -108.0000000000000284, 0.000000000000000000, 0.000000000000000000 ) ) ;
#9582 = CARTESIAN_POINT ( 'NONE',  ( 13.59724543428031573, 4.619798703722006294, -0.06738800180213055935 ) ) ;
#9583 = AXIS2_PLACEMENT_3D ( 'NONE', #6937, #2036, #9228 ) ;
#9584 = EDGE_CURVE ( 'NONE', #8413, #9967, #8604, .T. ) ;
#9585 = CARTESIAN_POINT ( 'NONE',  ( 11.92174236212692229, 7.340858601238088532, 11.71832628391215181 ) ) ;
#9586 = EDGE_LOOP ( 'NONE', ( #7361, #10011 ) ) ;
#9587 = CARTESIAN_POINT ( 'NONE',  ( 0.2000000000000057288, 4.286263797015736595E-16, -3.500000000000000000 ) ) ;
#9588 = CARTESIAN_POINT ( 'NONE',  ( 13.89598863503046111, -8.731428362939032795, 44.78571428571428470 ) ) ;
#9589 = CARTESIAN_POINT ( 'NONE',  ( -9.511495879682431411E-16, 20.00000000000000000, 0.000000000000000000 ) ) ;
#9590 = DIRECTION ( 'NONE',  ( 0.000000000000000000, -6.338944243255235518E-49, 1.000000000000000000 ) ) ;
#9591 = CIRCLE ( 'NONE', #499, 16.00000000000000000 ) ;
#9592 = CIRCLE ( 'NONE', #4792, 0.4999999999999994449 ) ;
#9593 = CARTESIAN_POINT ( 'NONE',  ( -9.865911304835474738, -1.562606840307925626, 14.55000000000000249 ) ) ;
#9594 = CARTESIAN_POINT ( 'NONE',  ( -1.486127417882243895, 9.383039235653825472, 6.299999999999972289 ) ) ;
#9595 = DIRECTION ( 'NONE',  ( 0.7063021515967569108, 0.7063021515967621289, -0.04769215134145721874 ) ) ;
#9596 = CARTESIAN_POINT ( 'NONE',  ( 5.164528828830335705, -15.14410076328347543, 31.43261199819787421 ) ) ;
#9597 = CARTESIAN_POINT ( 'NONE',  ( 56.99999999999997158, 0.000000000000000000, 0.000000000000000000 ) ) ;
#9598 = CARTESIAN_POINT ( 'NONE',  ( 13.82664651025767100, -8.841785722321541030, 36.78975485534072476 ) ) ;
#9599 = AXIS2_PLACEMENT_3D ( 'NONE', #8872, #1836, #1786 ) ;
#9600 = AXIS2_PLACEMENT_3D ( 'NONE', #10002, #3694, #1317 ) ;
#9601 = ADVANCED_FACE ( 'NONE', ( #2331 ), #8584, .T. ) ;
#9602 = AXIS2_PLACEMENT_3D ( 'NONE', #4083, #6394, #1715 ) ;
#9603 = EDGE_LOOP ( 'NONE', ( #3454, #7649, #8133, #8680 ) ) ;
#9604 = CARTESIAN_POINT ( 'NONE',  ( -16.30827793483735988, 1.837501619626141780, 29.35714285714285765 ) ) ;
#9605 = CARTESIAN_POINT ( 'NONE',  ( 3.725403445246824319, 14.71619381621854927, 7.152024097607907747E-17 ) ) ;
#9606 = CARTESIAN_POINT ( 'NONE',  ( -1.837501619626328297, 16.30827793483733856, 6.642857142857143238 ) ) ;
#9607 = CARTESIAN_POINT ( 'NONE',  ( -88.00000000000002842, 0.000000000000000000, 0.000000000000000000 ) ) ;
#9608 = SURFACE_SIDE_STYLE ('',( #5661 ) ) ;
#9609 = CARTESIAN_POINT ( 'NONE',  ( 4.270415729527831772, 8.486213763410694000, 10.59886208192144075 ) ) ;
#9610 = CARTESIAN_POINT ( 'NONE',  ( 7.771249796623105333, 7.842167650704658932, 19.74886208192143044 ) ) ;
#9611 = EDGE_CURVE ( 'NONE', #5816, #7640, #843, .T. ) ;
#9612 = AXIS2_PLACEMENT_3D ( 'NONE', #706, #3016, #853 ) ;
#9613 = CARTESIAN_POINT ( 'NONE',  ( 14.25515036105622535, -1.737328882695210241, 42.36118342676930126 ) ) ;
#9614 = CARTESIAN_POINT ( 'NONE',  ( -5.420364854931999155, -15.49051278174644253, 22.07142857142858006 ) ) ;
#9615 = CARTESIAN_POINT ( 'NONE',  ( 13.91197093850538380, 1.567502665446386390, 38.14285714285714590 ) ) ;
#9616 = CARTESIAN_POINT ( 'NONE',  ( 1.693770420379222319, 13.89774397934251837, 46.86118342676930126 ) ) ;
#9617 = CARTESIAN_POINT ( 'NONE',  ( 4.742819248065503146, 13.55419868402813677, 7.071428571428569398 ) ) ;
#9618 = CARTESIAN_POINT ( 'NONE',  ( 7.063212654743468377, 7.063212654743559860, 18.74999999999998934 ) ) ;
#9619 = CARTESIAN_POINT ( 'NONE',  ( -9.859792900771106261, 4.967534682030611215, 3.848862081921410105 ) ) ;
#9620 = ORIENTED_EDGE ( 'NONE', *, *, #9121, .F. ) ;
#9621 = CARTESIAN_POINT ( 'NONE',  ( -1.737328882695368115, 14.25515036105620581, 50.63881657323071295 ) ) ;
#9622 = ORIENTED_EDGE ( 'NONE', *, *, #4219, .T. ) ;
#9623 = CYLINDRICAL_SURFACE ( 'NONE', #6778, 8.200000000000009948 ) ;
#9624 = CARTESIAN_POINT ( 'NONE',  ( -15.10213328493390961, 5.284464991282586510, 23.57142857142857650 ) ) ;
#9625 = CARTESIAN_POINT ( 'NONE',  ( -13.47998361472151174, -8.620103694222146729, 36.71024514465928235 ) ) ;
#9626 = CARTESIAN_POINT ( 'NONE',  ( 10.37072757624895836, -1.642561882922356498, 13.19999999999998863 ) ) ;
#9627 = CARTESIAN_POINT ( 'NONE',  ( 5.012215536711511987, -9.837026868205997587, 7.649999999999992362 ) ) ;
#9628 = LINE ( 'NONE', #7959, #8262 ) ;
#9629 = ORIENTED_EDGE ( 'NONE', *, *, #9823, .T. ) ;
#9630 = CARTESIAN_POINT ( 'NONE',  ( -4.743843029824828861, 13.17239914596749450, 20.42453085894499054 ) ) ;
#9631 = CARTESIAN_POINT ( 'NONE',  ( -4.766900247265192014, -9.355568503977867323, 11.09999999999999787 ) ) ;
#9632 = CARTESIAN_POINT ( 'NONE',  ( -1.791431617652833763, -15.89939535829188877, 9.857142857142855874 ) ) ;
#9633 = FACE_BOUND ( 'NONE', #664, .T. ) ;
#9634 = CARTESIAN_POINT ( 'NONE',  ( -4.619798703721853528, -13.59724543428036725, 42.06738800180214355 ) ) ;
#9635 = CARTESIAN_POINT ( 'NONE',  ( -1.595456901104623348, 10.37818827243066622, 11.30113791807855961 ) ) ;
#9636 = CARTESIAN_POINT ( 'NONE',  ( -8.486213763410637156, -4.270415729527911708, 13.40113791807857702 ) ) ;
#9637 = DIRECTION ( 'NONE',  ( 4.755747939841215952E-17, -1.000000000000000000, 0.000000000000000000 ) ) ;
#9638 = CARTESIAN_POINT ( 'NONE',  ( 1.478298951650704351, -14.28433602490913579, 19.64689771248358596 ) ) ;
#9639 =( REPRESENTATION_RELATIONSHIP ('NONE','NONE', #58, #10217 ) REPRESENTATION_RELATIONSHIP_WITH_TRANSFORMATION ( #3869 )SHAPE_REPRESENTATION_RELATIONSHIP( ) );
#9640 = CARTESIAN_POINT ( 'NONE',  ( 13.17239914596754424, -4.743843029824685864, 12.57546914105500768 ) ) ;
#9641 = ORIENTED_EDGE ( 'NONE', *, *, #2743, .T. ) ;
#9642 = DIRECTION ( 'NONE',  ( 1.000000000000000000, 0.000000000000000000, 0.000000000000000000 ) ) ;
#9643 = CARTESIAN_POINT ( 'NONE',  ( -1.967016585148659846, 16.29368510291087091, 14.63881657323070939 ) ) ;
#9644 = DIRECTION ( 'NONE',  ( 1.000000000000000000, 4.755747939841215952E-17, -0.000000000000000000 ) ) ;
#9645 = CARTESIAN_POINT ( 'NONE',  ( -163.5777460020251795, -1.618434078064680870, 14.91276646089121627 ) ) ;
#9646 = CARTESIAN_POINT ( 'NONE',  ( 9.375578539472099848, -1.533232399699986370, 9.201137918078538647 ) ) ;
#9647 = CARTESIAN_POINT ( 'NONE',  ( -1.562606840307830591, -9.865911304835478290, 1.949999999999996181 ) ) ;
#9648 = CARTESIAN_POINT ( 'NONE',  ( -164.4416275561781333, 2.080988465785847286, 12.83239121171710018 ) ) ;
#9649 = CARTESIAN_POINT ( 'NONE',  ( 14.26974319298268767, -1.607813917172876916, 32.35714285714286120 ) ) ;
#9650 = CARTESIAN_POINT ( 'NONE',  ( 1.917699372585825790, 15.88516839912900203, 34.86118342676929416 ) ) ;
#9651 = ORIENTED_EDGE ( 'NONE', *, *, #7128, .T. ) ;
#9652 = EDGE_CURVE ( 'NONE', #7869, #1613, #685, .T. ) ;
#9653 = AXIS2_PLACEMENT_3D ( 'NONE', #8117, #2631, #2586 ) ;
#9654 = CARTESIAN_POINT ( 'NONE',  ( 16.30827793483735633, -1.837501619626142890, 26.35714285714285765 ) ) ;
#9655 = LINE ( 'NONE', #129, #8763 ) ;
#9656 = CARTESIAN_POINT ( 'NONE',  ( 5.284464991282756152, -15.10213328493384743, 15.42857142857143060 ) ) ;
#9657 = FILL_AREA_STYLE ('',( #3342 ) ) ;
#9658 = CARTESIAN_POINT ( 'NONE',  ( -1.677562661911643938, -10.91227292449344688, 14.94886208192145105 ) ) ;
#9659 = CARTESIAN_POINT ( 'NONE',  ( -4.503970704919988854, 13.25633410266674517, 46.43261199819787066 ) ) ;
#9660 = CARTESIAN_POINT ( 'NONE',  ( -1.791431617652833763, -15.89939535829188877, 15.85714285714286120 ) ) ;
#9661 =( LENGTH_UNIT ( ) NAMED_UNIT ( * ) SI_UNIT ( .MILLI., .METRE. ) );
#9662 = CARTESIAN_POINT ( 'NONE',  ( 7.556039541191335474, 11.78653521626503320, 41.28975485534072476 ) ) ;
#9663 = CARTESIAN_POINT ( 'NONE',  ( 10.15407889436379030, 10.15407889436390576, 13.50000000000000178 ) ) ;
#9664 = CARTESIAN_POINT ( 'NONE',  ( 1.562606840307832146, 9.865911304835501383, 18.44999999999999929 ) ) ;
#9665 = CARTESIAN_POINT ( 'NONE',  ( -9.859792900771106261, 4.967534682030606774, 6.848862081921402556 ) ) ;
#9666 = VERTEX_POINT ( 'NONE', #579 ) ;
#9667 = CARTESIAN_POINT ( 'NONE',  ( 7.639999817571789364, -12.15899005565156266, 3.214285714285716633 ) ) ;
#9668 = EDGE_LOOP ( 'NONE', ( #6409, #4753, #4443, #7933 ) ) ;
#9669 = DIRECTION ( 'NONE',  ( 0.7071067811865519026, -0.7071067811865431318, 0.000000000000000000 ) ) ;
#9670 = CARTESIAN_POINT ( 'NONE',  ( 15.89939535829187278, 1.791431617653015174, 14.14285714285714413 ) ) ;
#9671 = CARTESIAN_POINT ( 'NONE',  ( 15.88516839912898071, 1.917699372586004092, 34.13881657323070584 ) ) ;
#9672 = CARTESIAN_POINT ( 'NONE',  ( 1.727091770866550968, 10.90442828429187294, 9.449999999999988631 ) ) ;
#9673 = CARTESIAN_POINT ( 'NONE',  ( 7.424621202458790314, -7.424621202458697944, 10.50000000000000888 ) ) ;
#9674 = LINE ( 'NONE', #7135, #3644 ) ;
#9675 = CARTESIAN_POINT ( 'NONE',  ( -4.619798703721853528, -13.59724543428036725, 12.06738800180214000 ) ) ;
#9676 = ORIENTED_EDGE ( 'NONE', *, *, #10033, .T. ) ;
#9677 = CARTESIAN_POINT ( 'NONE',  ( 9.355568503977840678, 4.766900247265305701, 15.90000000000002522 ) ) ;
#9678 = CARTESIAN_POINT ( 'NONE',  ( -15.49051278174638036, -5.420364854932175902, 16.92857142857143771 ) ) ;
#9679 = DIRECTION ( 'NONE',  ( 0.000000000000000000, 1.000000000000000000, 0.000000000000000000 ) ) ;
#9680 = CARTESIAN_POINT ( 'NONE',  ( 9.989344678689365153, -9.809645194533958446, 40.99595943037355994 ) ) ;
#9681 = CARTESIAN_POINT ( 'NONE',  ( -9.377220287598998283, -4.724406229267462898, 10.40113791807857524 ) ) ;
#9682 = CARTESIAN_POINT ( 'NONE',  ( -7.842167650704559456, -7.771249796623176387, 1.251137918078559563 ) ) ;
#9683 = DIRECTION ( 'NONE',  ( 0.000000000000000000, 8.191099868251448390E-34, 1.000000000000000000 ) ) ;
#9684 =( NAMED_UNIT ( * ) SI_UNIT ( $, .STERADIAN. ) SOLID_ANGLE_UNIT ( ) );
#9685 = LINE ( 'NONE', #6410, #5870 ) ;
#9686 = ADVANCED_BREP_SHAPE_REPRESENTATION ( '', ( #7117, #3995 ), #10094 ) ;
#9687 = CARTESIAN_POINT ( 'NONE',  ( 15.88516839912898071, 1.917699372586004092, 4.138816573230708507 ) ) ;
#9688 = DIRECTION ( 'NONE',  ( 0.000000000000000000, 0.000000000000000000, 1.000000000000000000 ) ) ;
#9689 = DIRECTION ( 'NONE',  ( 1.000000000000000000, 0.000000000000000000, 0.000000000000000000 ) ) ;
#9690 = CARTESIAN_POINT ( 'NONE',  ( -8.486213763410637156, -4.270415729527911708, 4.401137918078569022 ) ) ;
#9691 = CARTESIAN_POINT ( 'NONE',  ( 1.486127417882244783, -9.383039235653791721, 1.800000000000023803 ) ) ;
#9692 = EDGE_CURVE ( 'NONE', #2970, #5864, #5462, .T. ) ;
#9693 = CARTESIAN_POINT ( 'NONE',  ( -162.9599602851104976, 0.6932240239557875272, 12.98215789948331889 ) ) ;
#9694 = CARTESIAN_POINT ( 'NONE',  ( 12.15899005565164792, -7.639999817571655250, 32.78571428571430602 ) ) ;
#9695 = CARTESIAN_POINT ( 'NONE',  ( 15.06016580658428694, -5.404401153735007846, 42.57546914105501656 ) ) ;
#9696 = MECHANICAL_DESIGN_GEOMETRIC_PRESENTATION_REPRESENTATION (  '', ( #2590 ), #7378 ) ;
#9697 = ORIENTED_EDGE ( 'NONE', *, *, #8641, .T. ) ;
#9698 = CARTESIAN_POINT ( 'NONE',  ( -1.791431617652833763, -15.89939535829188877, 27.85714285714285765 ) ) ;
#9699 = CARTESIAN_POINT ( 'NONE',  ( 3.907812701641489639, 14.44795834638319398, 1.336143574212688912E-16 ) ) ;
#9700 = CARTESIAN_POINT ( 'NONE',  ( -13.54758718765249625, -8.512513224245459753, 16.71428571428571530 ) ) ;
#9701 = DIRECTION ( 'NONE',  ( -2.311115933264683708E-33, 1.040834085586086106E-16, 1.000000000000000000 ) ) ;
#9702 = CARTESIAN_POINT ( 'NONE',  ( 7.027753727702739539, 7.098671581784283369, 13.74886208192144643 ) ) ;
#9703 = CARTESIAN_POINT ( 'NONE',  ( 5.056896391392317724, -9.814260835640970626, 17.64886208192141126 ) ) ;
#9704 = UNCERTAINTY_MEASURE_WITH_UNIT (LENGTH_MEASURE( 1.000000000000000082E-05 ), #5689, 'distance_accuracy_value', 'NONE');
#9705 = CARTESIAN_POINT ( 'NONE',  ( 1.917699372585825790, 15.88516839912900203, 10.86118342676929238 ) ) ;
#9706 = CARTESIAN_POINT ( 'NONE',  ( -13.89598863503046111, 8.731428362939027465, 29.78571428571428825 ) ) ;
#9707 = CYLINDRICAL_SURFACE ( 'NONE', #1180, 15.00000000000000000 ) ;
#9708 = PRESENTATION_LAYER_ASSIGNMENT (  '', '', ( #4253 ) ) ;
#9709 = CARTESIAN_POINT ( 'NONE',  ( 13.82664651025767100, -8.841785722321541030, 0.7897548553407187644 ) ) ;
#9710 = CARTESIAN_POINT ( 'NONE',  ( -14.26974319298268767, 1.607813917172874918, 17.35714285714286476 ) ) ;
#9711 = EDGE_CURVE ( 'NONE', #2369, #8072, #3724, .T. ) ;
#9712 = FACE_OUTER_BOUND ( 'NONE', #9668, .T. ) ;
#9713 = CARTESIAN_POINT ( 'NONE',  ( 9.859792900771104485, -4.967534682030585458, 5.348862081921449629 ) ) ;
#9714 = VERTEX_POINT ( 'NONE', #4507 ) ;
#9715 = CARTESIAN_POINT ( 'NONE',  ( -13.55419868402807992, -4.742819248065651472, 22.92857142857142705 ) ) ;
#9716 = ORIENTED_EDGE ( 'NONE', *, *, #7905, .F. ) ;
#9717 = DIRECTION ( 'NONE',  ( 0.000000000000000000, 8.191099868251446680E-34, 1.000000000000000000 ) ) ;
#9718 = CARTESIAN_POINT ( 'NONE',  ( -1.791431617652833763, -15.89939535829188877, 27.85714285714285765 ) ) ;
#9719 = CARTESIAN_POINT ( 'NONE',  ( 8.404922754268618235, 13.61519076058357491, 39.28167371608785174 ) ) ;
#9720 = CARTESIAN_POINT ( 'NONE',  ( -1.727091770866549414, -10.90442828429184630, 10.95000000000000462 ) ) ;
#9721 = CARTESIAN_POINT ( 'NONE',  ( 9.355568503977840678, 4.766900247265305701, 18.90000000000002700 ) ) ;
#9722 = CARTESIAN_POINT ( 'NONE',  ( 12.15899005565164792, -7.639999817571654361, 14.78571428571429180 ) ) ;
#9723 = ADVANCED_FACE ( 'NONE', ( #8484 ), #6142, .F. ) ;
#9724 = ORIENTED_EDGE ( 'NONE', *, *, #2412, .T. ) ;
#9725 = CARTESIAN_POINT ( 'NONE',  ( -9.989344678689363377, 9.809645194533960222, 31.99595943037357060 ) ) ;
#9726 = ORIENTED_EDGE ( 'NONE', *, *, #3204, .T. ) ;
#9727 = CARTESIAN_POINT ( 'NONE',  ( 7.806708723663832394, 7.806708723663931870, 18.74999999999998934 ) ) ;
#9728 = CARTESIAN_POINT ( 'NONE',  ( -11.60466159355861926, -11.60466159355875249, 16.50000000000000000 ) ) ;
#9729 = PRODUCT_RELATED_PRODUCT_CATEGORY ( 'part', '', ( #9151 ) ) ;
#9730 = CARTESIAN_POINT ( 'NONE',  ( -170.0000000000000284, 12.99999999999999289, 0.000000000000000000 ) ) ;
#9731 = CARTESIAN_POINT ( 'NONE',  ( 14.28433602490915000, -1.478298951650544479, 40.35310228751642825 ) ) ;
#9732 = CARTESIAN_POINT ( 'NONE',  ( -1.642561882922479732, 10.37072757624895303, 0.2999999999999669598 ) ) ;
#9733 = CARTESIAN_POINT ( 'NONE',  ( -10.91227292449344155, -1.677562661911747632, 1.551137918078593803 ) ) ;
#9734 = CARTESIAN_POINT ( 'NONE',  ( -108.0000000000000284, 1.959434878635764737E-15, -15.99999999999999645 ) ) ;
#9735 = CARTESIAN_POINT ( 'NONE',  ( -1.693770420379220099, -13.89774397934251837, 13.86118342676929416 ) ) ;
#9736 = CARTESIAN_POINT ( 'NONE',  ( 11.92174236212692229, 7.340858601238088532, 23.71832628391215181 ) ) ;
#9737 = CARTESIAN_POINT ( 'NONE',  ( 5.012215536711511987, -9.837026868205999364, 10.65000000000000924 ) ) ;
#9738 = CARTESIAN_POINT ( 'NONE',  ( 11.09109556827038467, 11.02177121192640818, 48.73000000000001819 ) ) ;
#9739 = CARTESIAN_POINT ( 'NONE',  ( -5.404401153735176599, 15.06016580658422477, 8.424530858944992318 ) ) ;
#9740 = DIRECTION ( 'NONE',  ( 0.000000000000000000, -6.338944243255235518E-49, 1.000000000000000000 ) ) ;
#9741 = FACE_OUTER_BOUND ( 'NONE', #10034, .T. ) ;
#9743 =( GEOMETRIC_REPRESENTATION_CONTEXT ( 3 ) GLOBAL_UNCERTAINTY_ASSIGNED_CONTEXT ( ( #6670 ) ) GLOBAL_UNIT_ASSIGNED_CONTEXT ( ( #7797, #7836, #5458 ) ) REPRESENTATION_CONTEXT ( 'NONE', 'WORKASPACE' ) );
#9742 = CARTESIAN_POINT ( 'NONE',  ( 4.312909747525650594, 8.464561979789532842, 18.60000000000000497 ) ) ;
#9744 = CARTESIAN_POINT ( 'NONE',  ( -162.8640756141387840, 0.2830513900230973712, 14.99796416534026200 ) ) ;
#9745 = CARTESIAN_POINT ( 'NONE',  ( -13.21436662431716869, 4.623906867372262752, 35.57142857142857650 ) ) ;
#9746 = ADVANCED_FACE ( 'NONE', ( #7027 ), #3050, .T. ) ;
#9747 = CARTESIAN_POINT ( 'NONE',  ( 12.15899005565164792, -7.639999817571655250, 32.78571428571430602 ) ) ;
#9748 = VERTEX_POINT ( 'NONE', #6913 ) ;
#9749 = AXIS2_PLACEMENT_3D ( 'NONE', #3245, #3294, #2669 ) ;
#9750 = CARTESIAN_POINT ( 'NONE',  ( 11.31370849898482334, -11.31370849898469366, 33.00000000000000000 ) ) ;
#9751 = CARTESIAN_POINT ( 'NONE',  ( 7.071067811865515473, -7.071067811865425767, 19.50000000000001776 ) ) ;
#9752 = AXIS2_PLACEMENT_3D ( 'NONE', #4356, #5798, #1252 ) ;
#9753 = CARTESIAN_POINT ( 'NONE',  ( -13.89598863503046111, 8.731428362939027465, 17.78571428571428115 ) ) ;
#9754 = PRESENTATION_STYLE_ASSIGNMENT (( #3434 ) ) ;
#9755 = CARTESIAN_POINT ( 'NONE',  ( -6.751237864895158758, 6.683790977649261222, 18.99886208192142334 ) ) ;
#9756 = CARTESIAN_POINT ( 'NONE',  ( -7.027753727702738651, -7.098671581784262941, 6.248862081921465084 ) ) ;
#9757 = CARTESIAN_POINT ( 'NONE',  ( -15.53355953199861794, -5.297344310588530725, 14.93261199819787066 ) ) ;
#9758 = CIRCLE ( 'NONE', #1670, 1.816100000000000270 ) ;
#9759 = CARTESIAN_POINT ( 'NONE',  ( -15.10213328493390961, 5.284464991282586510, 35.57142857142857650 ) ) ;
#9760 = AXIS2_PLACEMENT_3D ( 'NONE', #4993, #1165, #9902 ) ;
#9761 = AXIS2_PLACEMENT_3D ( 'NONE', #5220, #1099, #1052 ) ;
#9762 = PRESENTATION_STYLE_ASSIGNMENT (( #4220 ) ) ;
#9763 = CARTESIAN_POINT ( 'NONE',  ( -11.69682198916834892, -11.51250119794901394, 2.504040569626438728 ) ) ;
#9764 = CARTESIAN_POINT ( 'NONE',  ( -11.85413878919593422, -7.448449071214776396, 10.71428571428571708 ) ) ;
#9765 = FACE_OUTER_BOUND ( 'NONE', #438, .T. ) ;
#9766 = CARTESIAN_POINT ( 'NONE',  ( -10.89658364409024749, -1.776620879821561694, 3.548862081921419609 ) ) ;
#9767 = EDGE_LOOP ( 'NONE', ( #7209, #4652 ) ) ;
#9768 = CARTESIAN_POINT ( 'NONE',  ( -14.26974319298268767, 1.607813917172874918, 17.35714285714286476 ) ) ;
#9769 = ORIENTED_EDGE ( 'NONE', *, *, #9692, .F. ) ;
#9770 = AXIS2_PLACEMENT_3D ( 'NONE', #6649, #472, #6744 ) ;
#9771 = CARTESIAN_POINT ( 'NONE',  ( -5.420364854931998266, -15.49051278174643898, 28.07142857142857295 ) ) ;
#9772 = CARTESIAN_POINT ( 'NONE',  ( 1.967016585148662289, -16.29368510291087091, 35.63881657323071295 ) ) ;
#9773 = CARTESIAN_POINT ( 'NONE',  ( 7.806708723663831506, 7.806708723663925653, 9.749999999999982236 ) ) ;
#9774 = EDGE_CURVE ( 'NONE', #1035, #5632, #10185, .T. ) ;
#9775 = CARTESIAN_POINT ( 'NONE',  ( -13.55419868402807992, -4.742819248065651472, 4.928571428571430602 ) ) ;
#9776 = MECHANICAL_DESIGN_GEOMETRIC_PRESENTATION_REPRESENTATION (  '', ( #4486 ), #1352 ) ;
#9777 = ORIENTED_EDGE ( 'NONE', *, *, #8156, .T. ) ;
#9778 = EDGE_CURVE ( 'NONE', #9861, #1810, #5328, .T. ) ;
#9779 = CARTESIAN_POINT ( 'NONE',  ( 4.743843029824831525, -13.17239914596749095, 29.42453085894499765 ) ) ;
#9780 = EDGE_LOOP ( 'NONE', ( #5025, #9382 ) ) ;
#9781 = FILL_AREA_STYLE ('',( #8208 ) ) ;
#9782 = CARTESIAN_POINT ( 'NONE',  ( 7.042703574009315126, 12.29825027030509865, 48.73000000000005372 ) ) ;
#9783 = CARTESIAN_POINT ( 'NONE',  ( -9.989344678689363377, 9.809645194533960222, 37.99595943037355994 ) ) ;
#9784 = AXIS2_PLACEMENT_3D ( 'NONE', #6442, #2755, #5900 ) ;
#9785 = CARTESIAN_POINT ( 'NONE',  ( -9.377220287598998283, -4.724406229267462898, 13.40113791807857702 ) ) ;
#9786 = CARTESIAN_POINT ( 'NONE',  ( 1.776620879821457333, 10.89658364409028124, 5.451137918078557298 ) ) ;
#9787 = LINE ( 'NONE', #2689, #5624 ) ;
#9788 = CARTESIAN_POINT ( 'NONE',  ( -13.17239914596754424, 4.743843029824683200, 15.57546914105500413 ) ) ;
#9789 = FILL_AREA_STYLE ('',( #4399 ) ) ;
#9790 = CARTESIAN_POINT ( 'NONE',  ( 10.90442828429183919, 1.727091770866679310, 7.050000000000010481 ) ) ;
#9791 = CARTESIAN_POINT ( 'NONE',  ( 1.665163862719847732, 15.91362231745477374, 38.85310228751641404 ) ) ;
#9792 = EDGE_CURVE ( 'NONE', #3268, #9145, #3475, .T. ) ;
#9793 = CARTESIAN_POINT ( 'NONE',  ( -10.36771240197842303, 11.87284897423499785, 48.72999999999976239 ) ) ;
#9794 = CARTESIAN_POINT ( 'NONE',  ( 5.404401153735178376, -15.06016580658422477, 5.424530858944991429 ) ) ;
#9795 = DIRECTION ( 'NONE',  ( -1.000000000000000000, 1.842239752758738928E-31, -1.780435181894459419E-32 ) ) ;
#9796 = CARTESIAN_POINT ( 'NONE',  ( -8.877401133907129704, 4.579542530753039742, 1.851137918078540334 ) ) ;
#9797 = CARTESIAN_POINT ( 'NONE',  ( -9.865911304835474738, -1.562606840307925626, 17.55000000000002913 ) ) ;
#9798 = CARTESIAN_POINT ( 'NONE',  ( -1.925929944387235853E-31, -1.018491042385001544, -1.270000000000007123 ) ) ;
#9799 = CARTESIAN_POINT ( 'NONE',  ( 7.639999817571789364, -12.15899005565156266, 27.21428571428572241 ) ) ;
#9800 = AXIS2_PLACEMENT_3D ( 'NONE', #3402, #3118, #6259 ) ;
#9801 = VERTEX_POINT ( 'NONE', #3781 ) ;
#9802 = CARTESIAN_POINT ( 'NONE',  ( 15.49051278174638036, 5.420364854932175014, 43.92857142857143060 ) ) ;
#9803 = DIRECTION ( 'NONE',  ( 0.000000000000000000, -6.338944243255235518E-49, 1.000000000000000000 ) ) ;
#9804 = CARTESIAN_POINT ( 'NONE',  ( -15.49051278174638036, -5.420364854932175902, 10.92857142857142883 ) ) ;
#9805 = PRODUCT ( 'small spring', 'small spring', '', ( #2009 ) ) ;
#9806 = DIRECTION ( 'NONE',  ( 0.000000000000000000, 6.938893903907220674E-18, 1.000000000000000000 ) ) ;
#9807 = CARTESIAN_POINT ( 'NONE',  ( -1.533232399700100057, 9.375578539472098072, 16.29886208192143471 ) ) ;
#9808 = CARTESIAN_POINT ( 'NONE',  ( -1.513077731352923339, -9.873755945037078874, 8.948862081921467038 ) ) ;
#9809 = PRODUCT_DEFINITION_CONTEXT ( 'detailed design', #6045, 'design' ) ;
#9810 = CARTESIAN_POINT ( 'NONE',  ( 11.22385875690717683, -11.40355824106234373, 13.00404056962644006 ) ) ;
#9811 = CARTESIAN_POINT ( 'NONE',  ( 1.837501619626330074, -16.30827793483733501, 27.64285714285714590 ) ) ;
#9812 =( NAMED_UNIT ( * ) SI_UNIT ( $, .STERADIAN. ) SOLID_ANGLE_UNIT ( ) );
#9813 = CARTESIAN_POINT ( 'NONE',  ( 11.69682198916835070, 11.51250119794901394, -0.4959594303735606058 ) ) ;
#9814 = CARTESIAN_POINT ( 'NONE',  ( 7.639999817571789364, -12.15899005565156266, 27.21428571428572241 ) ) ;
#9815 = CARTESIAN_POINT ( 'NONE',  ( -1.791431617652833763, -15.89939535829188877, 9.857142857142855874 ) ) ;
#9816 = CARTESIAN_POINT ( 'NONE',  ( -5.056896391392315948, 9.814260835640991942, 4.148862081921444123 ) ) ;
#9817 = VERTEX_POINT ( 'NONE', #5426 ) ;
#9818 = CARTESIAN_POINT ( 'NONE',  ( 4.742819248065503146, 13.55419868402813677, 13.07142857142857295 ) ) ;
#9819 = ORIENTED_EDGE ( 'NONE', *, *, #5443, .F. ) ;
#9820 = CARTESIAN_POINT ( 'NONE',  ( -15.10213328493390961, 5.284464991282586510, 35.57142857142857650 ) ) ;
#9821 = CARTESIAN_POINT ( 'NONE',  ( 14.28433602490915000, -1.478298951650544479, 4.353102287516421143 ) ) ;
#9822 = CARTESIAN_POINT ( 'NONE',  ( 10.90442828429183919, 1.727091770866679532, 16.04999999999995808 ) ) ;
#9823 = EDGE_CURVE ( 'NONE', #1651, #9748, #8765, .T. ) ;
#9824 = CARTESIAN_POINT ( 'NONE',  ( -11.85413878919593422, -7.448449071214776396, 16.71428571428571530 ) ) ;
#9825 = CARTESIAN_POINT ( 'NONE',  ( 10.06191849875406064, 10.24623928997363187, 27.49595943037356705 ) ) ;
#9826 = ORIENTED_EDGE ( 'NONE', *, *, #4236, .F. ) ;
#9827 = DIRECTION ( 'NONE',  ( 0.000000000000000000, 6.338944243255235518E-49, -1.000000000000000000 ) ) ;
#9828 = CARTESIAN_POINT ( 'NONE',  ( 4.000000000000003553, 4.286263797015736595E-16, -3.500000000000000000 ) ) ;
#9829 =( REPRESENTATION_RELATIONSHIP ('NONE','NONE', #58, #1843 ) REPRESENTATION_RELATIONSHIP_WITH_TRANSFORMATION ( #873 )SHAPE_REPRESENTATION_RELATIONSHIP( ) );
#9830 = CARTESIAN_POINT ( 'NONE',  ( -9.390499931835536884, 1.439022436064298249, 3.698862081921452827 ) ) ;
#9831 = CARTESIAN_POINT ( 'NONE',  ( -11.78653521626494793, -7.556039541191465148, 48.71024514465926814 ) ) ;
#9832 = CARTESIAN_POINT ( 'NONE',  ( -10.91227292449344155, -1.677562661911747632, 16.55113791807855605 ) ) ;
#9833 = CARTESIAN_POINT ( 'NONE',  ( 9.377220287599001836, 4.724406229267489543, 5.901137918078571687 ) ) ;
#9834 = DIRECTION ( 'NONE',  ( -0.000000000000000000, 0.000000000000000000, 1.000000000000000000 ) ) ;
#9835 = CARTESIAN_POINT ( 'NONE',  ( -1.642561882922479732, 10.37072757624896191, 6.299999999999972289 ) ) ;
#9836 = CARTESIAN_POINT ( 'NONE',  ( -11.40355824106246807, 11.22385875690704715, 37.99595943037355994 ) ) ;
#9837 = ORIENTED_EDGE ( 'NONE', *, *, #7789, .T. ) ;
#9838 = CARTESIAN_POINT ( 'NONE',  ( -13.18366518639671625, 7.227486437412175668, 48.73000000000003240 ) ) ;
#9839 = CARTESIAN_POINT ( 'NONE',  ( -15.89939535829186923, -1.791431617653016062, 23.14285714285714590 ) ) ;
#9840 = DIRECTION ( 'NONE',  ( 0.000000000000000000, 0.000000000000000000, 1.000000000000000000 ) ) ;
#9841 = CARTESIAN_POINT ( 'NONE',  ( -7.098671581784199880, -7.027753727702809705, 4.251137918078595312 ) ) ;
#9842 = CARTESIAN_POINT ( 'NONE',  ( -7.063212654743466601, -7.063212654743531438, 11.24999999999999467 ) ) ;
#9843 = CARTESIAN_POINT ( 'NONE',  ( -164.3076905434401453, 2.040364482056596707, 14.86068217355785670 ) ) ;
#9844 = CARTESIAN_POINT ( 'NONE',  ( 1.707986654103998303, -16.32287076676380266, 37.64689771248358596 ) ) ;
#9845 = CARTESIAN_POINT ( 'NONE',  ( 7.448449071214646722, 11.85413878919601594, 25.28571428571428470 ) ) ;
#9846 = CARTESIAN_POINT ( 'NONE',  ( 13.91197093850538380, 1.567502665446386390, 44.14285714285714590 ) ) ;
#9847 = ORIENTED_EDGE ( 'NONE', *, *, #8243, .T. ) ;
#9848 = CARTESIAN_POINT ( 'NONE',  ( 8.404922754268618235, 13.61519076058357491, 3.281673716087854409 ) ) ;
#9849 = CARTESIAN_POINT ( 'NONE',  ( 2.826141341537784513, 15.12951547267378949, 6.336793937239309722E-15 ) ) ;
#9850 = CARTESIAN_POINT ( 'NONE',  ( 15.89939535829187278, 1.791431617653015174, 14.14285714285714413 ) ) ;
#9851 = FILL_AREA_STYLE_COLOUR ( '', #8426 ) ;
#9852 = CARTESIAN_POINT ( 'NONE',  ( -6.751237864895158758, 6.683790977649261222, 15.99886208192142512 ) ) ;
#9853 = CARTESIAN_POINT ( 'NONE',  ( -9.390499931835536884, 1.439022436064298249, 6.698862081921455491 ) ) ;
#9854 = CARTESIAN_POINT ( 'NONE',  ( -8.621071003556675549, 13.96533075980314642, 10.21832628391215358 ) ) ;
#9855 = CARTESIAN_POINT ( 'NONE',  ( -15.49051278174638036, -5.420364854932175902, 34.92857142857145192 ) ) ;
#9856 = VECTOR ( 'NONE', #8814, 1000.000000000000000 ) ;
#9857 = CARTESIAN_POINT ( 'NONE',  ( 11.69682198916835070, 11.51250119794901394, 11.50404056962644006 ) ) ;
#9858 = CARTESIAN_POINT ( 'NONE',  ( -10.15407889436378852, -10.15407889436390576, 22.50000000000000000 ) ) ;
#9859 = CARTESIAN_POINT ( 'NONE',  ( 13.89598863503046111, -8.731428362939032795, 2.785714285714284255 ) ) ;
#9860 = CARTESIAN_POINT ( 'NONE',  ( -8.731428362939189114, 13.89598863503036341, 42.21428571428572241 ) ) ;
#9861 = VERTEX_POINT ( 'NONE', #9419 ) ;
#9862 = CARTESIAN_POINT ( 'NONE',  ( -1.607813917173034124, 14.26974319298267524, 12.64285714285714235 ) ) ;
#9863 = ORIENTED_EDGE ( 'NONE', *, *, #6528, .F. ) ;
#9864 = AXIS2_PLACEMENT_3D ( 'NONE', #4500, #572, #10026 ) ;
#9865 = CARTESIAN_POINT ( 'NONE',  ( 5.420364854932000931, 15.49051278174644075, 37.07142857142857650 ) ) ;
#9866 = CARTESIAN_POINT ( 'NONE',  ( 11.51250119794888249, 11.69682198916847682, 45.49595943037356705 ) ) ;
#9867 = CARTESIAN_POINT ( 'NONE',  ( 9.837026868206066865, -5.012215536711392083, 13.34999999999998188 ) ) ;
#9868 = EDGE_CURVE ( 'NONE', #7540, #1499, #8373, .T. ) ;
#9869 = PRODUCT_CONTEXT ( 'NONE', #8770, 'mechanical' ) ;
#9870 = CARTESIAN_POINT ( 'NONE',  ( -11.85413878919593422, -7.448449071214776396, 10.71428571428571708 ) ) ;
#9871 = ADVANCED_FACE ( 'NONE', ( #152, #781 ), #3986, .F. ) ;
#9872 = CARTESIAN_POINT ( 'NONE',  ( 1.737328882695370558, -14.25515036105620581, 29.63881657323071295 ) ) ;
#9873 = ORIENTED_EDGE ( 'NONE', *, *, #6620, .T. ) ;
#9874 = CARTESIAN_POINT ( 'NONE',  ( 1.727091770866551412, 10.90442828429186761, 18.44999999999999929 ) ) ;
#9875 = CARTESIAN_POINT ( 'NONE',  ( -158.0000000000000284, 12.99999999999999645, 0.000000000000000000 ) ) ;
#9876 = CARTESIAN_POINT ( 'NONE',  ( 10.37818827243067510, -1.595456901104500780, 17.19886208192146171 ) ) ;
#9877 = CARTESIAN_POINT ( 'NONE',  ( -7.750357176954294935, 12.08964793087877787, 50.21024514465927524 ) ) ;
#9878 = CARTESIAN_POINT ( 'NONE',  ( -7.806708723663830618, -7.806708723663906113, 2.249999999999986233 ) ) ;
#9879 = CARTESIAN_POINT ( 'NONE',  ( 7.842167650704563897, 7.771249796623202144, 5.751137918078548239 ) ) ;
#9880 = CYLINDRICAL_SURFACE ( 'NONE', #10086, 16.99999999999997868 ) ;
#9881 = CARTESIAN_POINT ( 'NONE',  ( -13.92619789766827054, -1.441234910513399470, 27.14689771248358241 ) ) ;
#9882 = CARTESIAN_POINT ( 'NONE',  ( 0.000000000000000000, 0.000000000000000000, 0.000000000000000000 ) ) ;
#9883 = PRODUCT ( 'socket head cap screw_iso_ISO 4762 M4 x 10 - 10N', 'socket head cap screw_iso_ISO 4762 M4 x 10 - 10N', '', ( #4385 ) ) ;
#9884 = CARTESIAN_POINT ( 'NONE',  ( -1.727091770866549414, -10.90442828429184630, 10.95000000000000462 ) ) ;
#9885 = CARTESIAN_POINT ( 'NONE',  ( -11.51250119794888072, -11.69682198916848037, 36.49595943037355994 ) ) ;
#9886 = FACE_OUTER_BOUND ( 'NONE', #2115, .T. ) ;
#9887 = CARTESIAN_POINT ( 'NONE',  ( -13.89598863503046111, 8.731428362939027465, 23.78571428571429536 ) ) ;
#9888 = CARTESIAN_POINT ( 'NONE',  ( 4.000000000000007105, -1.802041971015319193E-33, -2.200000000000001066 ) ) ;
#9889 = CARTESIAN_POINT ( 'NONE',  ( 11.78653521626494793, 7.556039541191463371, 9.710245144659278793 ) ) ;
#9890 = CARTESIAN_POINT ( 'NONE',  ( -4.490180821391513533, 8.922933199037153429, 14.15113791807854327 ) ) ;
#9891 = CARTESIAN_POINT ( 'NONE',  ( 8.900167166472154889, -4.534861676072213577, 16.35000000000000497 ) ) ;
#9892 = PLANE ( 'NONE',  #1662 ) ;
#9893 = CARTESIAN_POINT ( 'NONE',  ( 7.448449071214646722, 11.85413878919601594, 49.28571428571428470 ) ) ;
#9894 = ADVANCED_FACE ( 'NONE', ( #8688 ), #3307, .F. ) ;
#9895 = CARTESIAN_POINT ( 'NONE',  ( -13.21436662431716869, 4.623906867372262752, 41.57142857142856940 ) ) ;
#9896 = VERTEX_POINT ( 'NONE', #8795 ) ;
#9897 = CARTESIAN_POINT ( 'NONE',  ( 13.89598863503046111, -8.731428362939032795, 38.78571428571429180 ) ) ;
#9898 = CARTESIAN_POINT ( 'NONE',  ( -158.0000000000000284, 12.99999999999999822, 0.000000000000000000 ) ) ;
#9899 = CARTESIAN_POINT ( 'NONE',  ( -8.731428362939189114, 13.89598863503036341, 30.21428571428572596 ) ) ;
#9900 = FACE_OUTER_BOUND ( 'NONE', #6642, .T. ) ;
#9901 = DIRECTION ( 'NONE',  ( 0.000000000000000000, 0.000000000000000000, 1.000000000000000000 ) ) ;
#9902 = DIRECTION ( 'NONE',  ( 0.000000000000000000, -8.191099868251446680E-34, -1.000000000000000000 ) ) ;
#9903 = CARTESIAN_POINT ( 'NONE',  ( 4.312909747525650594, 8.464561979789532842, 0.5999999999999894307 ) ) ;
#9904 = CARTESIAN_POINT ( 'NONE',  ( -7.027753727702738651, -7.098671581784268270, 3.248862081921429112 ) ) ;
#9905 = UNCERTAINTY_MEASURE_WITH_UNIT (LENGTH_MEASURE( 1.000000000000000082E-05 ), #5427, 'distance_accuracy_value', 'NONE');
#9906 = CARTESIAN_POINT ( 'NONE',  ( 4.766900247265192903, 9.355568503977902850, 15.60000000000000320 ) ) ;
#9907 = CARTESIAN_POINT ( 'NONE',  ( -11.22385875690717327, 11.40355824106234550, 10.00404056962643651 ) ) ;
#9908 = CARTESIAN_POINT ( 'NONE',  ( -11.31370849898482156, 11.31370849898469544, 24.00000000000000000 ) ) ;
#9909 = ADVANCED_FACE ( 'NONE', ( #1293 ), #4303, .T. ) ;
#9910 =( NAMED_UNIT ( * ) PLANE_ANGLE_UNIT ( ) SI_UNIT ( $, .RADIAN. ) );
#9911 = CARTESIAN_POINT ( 'NONE',  ( -15.06016580658428694, 5.404401153735006957, 3.575469141055005462 ) ) ;
#9912 = EDGE_CURVE ( 'NONE', #6462, #9103, #1833, .T. ) ;
#9913 = CARTESIAN_POINT ( 'NONE',  ( 12.15899005565164792, -7.639999817571655250, 26.78571428571429536 ) ) ;
#9914 = CARTESIAN_POINT ( 'NONE',  ( 13.54758718765249803, 8.512513224245457977, 7.714285714285715301 ) ) ;
#9915 = CARTESIAN_POINT ( 'NONE',  ( -11.60466159355861926, -11.60466159355875249, 40.50000000000000711 ) ) ;
#9916 = EDGE_LOOP ( 'NONE', ( #6787, #1905, #6335, #3689 ) ) ;
#9917 = CARTESIAN_POINT ( 'NONE',  ( -7.639999817571787588, 12.15899005565156266, 12.21428571428571885 ) ) ;
#9918 = CYLINDRICAL_SURFACE ( 'NONE', #6291, 2.149999999999985256 ) ;
#9919 = CARTESIAN_POINT ( 'NONE',  ( -15.49051278174637858, -5.420364854932175014, 28.92857142857143415 ) ) ;
#9920 = AXIS2_PLACEMENT_3D ( 'NONE', #2657, #8135, #7411 ) ;
#9921 = AXIS2_PLACEMENT_3D ( 'NONE', #5195, #1073, #1018 ) ;
#9922 = AXIS2_PLACEMENT_3D ( 'NONE', #1816, #218, #162 ) ;
#9923 = CARTESIAN_POINT ( 'NONE',  ( -13.96533075980324234, 8.621071003556515677, 49.78167371608785885 ) ) ;
#9924 = CARTESIAN_POINT ( 'NONE',  ( -7.771249796623103556, -7.842167650704637616, 3.248862081921429112 ) ) ;
#9925 = CARTESIAN_POINT ( 'NONE',  ( -4.623906867372410190, 13.21436662431711895, 30.42857142857143060 ) ) ;
#9926 = AXIS2_PLACEMENT_3D ( 'NONE', #6523, #9701, #7365 ) ;
#9927 = AXIS2_PLACEMENT_3D ( 'NONE', #4196, #8325, #7345 ) ;
#9928 = CARTESIAN_POINT ( 'NONE',  ( 9.989344678689365153, -9.809645194533958446, 28.99595943037357060 ) ) ;
#9929 = EDGE_LOOP ( 'NONE', ( #5691, #1368, #7918, #4178 ) ) ;
#9930 = DIRECTION ( 'NONE',  ( -1.000000000000000000, -1.387778780781445676E-16, -0.000000000000000000 ) ) ;
#9931 = CARTESIAN_POINT ( 'NONE',  ( 8.270439026029094975, 11.56191342138348332, 48.73000000000006082 ) ) ;
#9932 = CARTESIAN_POINT ( 'NONE',  ( 4.724406229267374968, 9.377220287599060455, 19.59886208192140700 ) ) ;
#9933 = EDGE_CURVE ( 'NONE', #6635, #3268, #9674, .T. ) ;
#9934 = CARTESIAN_POINT ( 'NONE',  ( 4.623906867372411078, -13.21436662431711717, 3.428571428571426605 ) ) ;
#9935 = CARTESIAN_POINT ( 'NONE',  ( -9.355568503977838901, -4.766900247265280832, 8.399999999999963052 ) ) ;
#9936 = CARTESIAN_POINT ( 'NONE',  ( -7.842167650704559456, -7.771249796623176387, 10.25113791807858021 ) ) ;
#9937 = FACE_OUTER_BOUND ( 'NONE', #1400, .T. ) ;
#9938 = CARTESIAN_POINT ( 'NONE',  ( -5.012215536711506658, 9.837026868206027785, 9.150000000000003908 ) ) ;
#9939 = CARTESIAN_POINT ( 'NONE',  ( -1.967016585148659846, 16.29368510291087091, 38.63881657323070584 ) ) ;
#9940 = CARTESIAN_POINT ( 'NONE',  ( -11.94288718622185641, 8.325416427328844904, 48.73000000000002530 ) ) ;
#9941 = VECTOR ( 'NONE', #7517, 1000.000000000000000 ) ;
#9942 = FACE_OUTER_BOUND ( 'NONE', #127, .T. ) ;
#9943 = CARTESIAN_POINT ( 'NONE',  ( 11.78653521626494793, 7.556039541191463371, 15.71024514465927879 ) ) ;
#9944 = CARTESIAN_POINT ( 'NONE',  ( 1.612135949262739398, 9.858066664633906129, 14.45113791807853509 ) ) ;
#9945 = CARTESIAN_POINT ( 'NONE',  ( -4.312909747525649706, -8.464561979789507973, 14.10000000000000142 ) ) ;
#9946 = CARTESIAN_POINT ( 'NONE',  ( -167.0812848797259562, 0.5571504444270253265, 14.99028060246901006 ) ) ;
#9947 = CARTESIAN_POINT ( 'NONE',  ( 4.865839792409144771, 13.51115193377589740, -0.9245308589449906522 ) ) ;
#9948 = PRODUCT_DEFINITION_SHAPE ( 'NONE', 'NONE',  #10237 ) ;
#9949 = CARTESIAN_POINT ( 'NONE',  ( 7.639999817571789364, -12.15899005565156266, 33.21428571428571530 ) ) ;
#9950 = ORIENTED_EDGE ( 'NONE', *, *, #8970, .T. ) ;
#9951 = CARTESIAN_POINT ( 'NONE',  ( 1.837501619626330074, -16.30827793483733501, 39.64285714285716722 ) ) ;
#9952 = DIRECTION ( 'NONE',  ( -1.000000000000000000, -0.000000000000000000, -0.000000000000000000 ) ) ;
#9953 = CARTESIAN_POINT ( 'NONE',  ( 8.512513224245308763, 13.54758718765259040, 31.28571428571428470 ) ) ;
#9954 = CARTESIAN_POINT ( 'NONE',  ( -6.976602070941134492, -13.58603705635637304, 0.000000000000000000 ) ) ;
#9955 = SURFACE_SIDE_STYLE ('',( #7518 ) ) ;
#9956 = VECTOR ( 'NONE', #8478, 1000.000000000000000 ) ;
#9957 = FACE_OUTER_BOUND ( 'NONE', #3759, .T. ) ;
#9958 = CARTESIAN_POINT ( 'NONE',  ( -8.464561979789474222, -4.312909747525728754, 5.400000000000016342 ) ) ;
#9959 = CARTESIAN_POINT ( 'NONE',  ( 7.027753727702739539, 7.098671581784288698, 10.74886208192140913 ) ) ;
#9960 = CARTESIAN_POINT ( 'NONE',  ( -7.806708723663830618, -7.806708723663901672, 11.24999999999999467 ) ) ;
#9961 = CARTESIAN_POINT ( 'NONE',  ( -16.30827793483735988, 1.837501619626141780, 41.35714285714286120 ) ) ;
#9962 = CARTESIAN_POINT ( 'NONE',  ( -1.707986654103994528, 16.32287076676380266, 22.64689771248357530 ) ) ;
#9963 = CARTESIAN_POINT ( 'NONE',  ( -15.89939535829186923, -1.791431617653016062, 11.14285714285714235 ) ) ;
#9964 = DIRECTION ( 'NONE',  ( -1.000000000000000000, 1.842239752758738928E-31, -1.780435181894459419E-32 ) ) ;
#9965 = ORIENTED_EDGE ( 'NONE', *, *, #863, .T. ) ;
#9966 = CARTESIAN_POINT ( 'NONE',  ( 1.727091770866550968, 10.90442828429187294, 15.44999999999997797 ) ) ;
#9967 = VERTEX_POINT ( 'NONE', #9477 ) ;
#9968 = CARTESIAN_POINT ( 'NONE',  ( 2.000000000000001776, 1.773042676681366281, 0.000000000000000000 ) ) ;
#9969 = CARTESIAN_POINT ( 'NONE',  ( 1.967016585148662289, -16.29368510291087091, 47.63881657323071295 ) ) ;
#9970 = CARTESIAN_POINT ( 'NONE',  ( -7.424621202458789426, 7.424621202458723701, 15.00000000000001421 ) ) ;
#9971 = CARTESIAN_POINT ( 'NONE',  ( -11.31370849898482156, 11.31370849898469544, 5.999999999999998224 ) ) ;
#9972 = SHAPE_DEFINITION_REPRESENTATION ( #5177, #8907 ) ;
#9973 = CARTESIAN_POINT ( 'NONE',  ( 4.623906867372411078, -13.21436662431711717, 21.42857142857142705 ) ) ;
#9974 = CARTESIAN_POINT ( 'NONE',  ( 7.340858601237956194, 11.92174236212700045, 45.28167371608785174 ) ) ;
#9975 = VECTOR ( 'NONE', #5111, 1000.000000000000000 ) ;
#9976 = ORIENTED_EDGE ( 'NONE', *, *, #7905, .T. ) ;
#9977 = DIRECTION ( 'NONE',  ( 0.2882273949230689802, 0.9575619921529161527, -1.755378125195851735E-33 ) ) ;
#9978 = CARTESIAN_POINT ( 'NONE',  ( -11.40355824106246807, 11.22385875690704715, 13.99595943037356527 ) ) ;
#9979 = LINE ( 'NONE', #1962, #9975 ) ;
#9980 = CARTESIAN_POINT ( 'NONE',  ( 8.922933199037192509, -4.490180821391404287, 5.348862081921449629 ) ) ;
#9981 = CARTESIAN_POINT ( 'NONE',  ( -1.607813917173034124, 14.26974319298267524, 0.6428571428571432378 ) ) ;
#9982 = CARTESIAN_POINT ( 'NONE',  ( -1.642561882922479732, 10.37072757624896191, 9.299999999999975842 ) ) ;
#9983 = CARTESIAN_POINT ( 'NONE',  ( -4.809394265263009061, -9.333916720356716823, 16.10113791807856742 ) ) ;
#9984 = DIRECTION ( 'NONE',  ( 0.000000000000000000, -6.338944243255235518E-49, 1.000000000000000000 ) ) ;
#9985 = CARTESIAN_POINT ( 'NONE',  ( 9.809645194534072132, -9.989344678689256796, 25.00404056962644006 ) ) ;
#9986 = ORIENTED_EDGE ( 'NONE', *, *, #7282, .F. ) ;
#9987 = CARTESIAN_POINT ( 'NONE',  ( 1.642561882922480621, -10.37072757624892638, 13.80000000000003446 ) ) ;
#9988 = CARTESIAN_POINT ( 'NONE',  ( 11.40355824106246985, -11.22385875690704538, 46.99595943037356705 ) ) ;
#9989 = CARTESIAN_POINT ( 'NONE',  ( -13.20914943391479390, 7.349713873783697338, 48.72999999999999687 ) ) ;
#9990 = CARTESIAN_POINT ( 'NONE',  ( 4.000000000000003553, 0.000000000000000000, 0.000000000000000000 ) ) ;
#9991 = CARTESIAN_POINT ( 'NONE',  ( 13.89774397934249706, 1.693770420379375308, 22.13881657323070939 ) ) ;
#9992 = CARTESIAN_POINT ( 'NONE',  ( 1.612135949262739398, 9.858066664633913234, 17.45113791807857240 ) ) ;
#9993 = CARTESIAN_POINT ( 'NONE',  ( -6.683790977649319842, 6.751237864895101026, 8.001137918078546463 ) ) ;
#9994 = CARTESIAN_POINT ( 'NONE',  ( -162.8500000000000512, -5.808233196467851957E-15, 13.00000000000000178 ) ) ;
#9995 = CARTESIAN_POINT ( 'NONE',  ( 1.567502665446232957, 13.91197093850540156, 48.85714285714286120 ) ) ;
#9996 = CARTESIAN_POINT ( 'NONE',  ( -9.809645194534070356, 9.989344678689256796, -1.995959430373561272 ) ) ;
#9997 = ORIENTED_EDGE ( 'NONE', *, *, #9349, .T. ) ;
#9998 = CARTESIAN_POINT ( 'NONE',  ( 15.10213328493390783, -5.284464991282587398, 38.57142857142857650 ) ) ;
#9999 = CARTESIAN_POINT ( 'NONE',  ( 0.000000000000000000, 0.000000000000000000, -1.270000000000007123 ) ) ;
#10000 = CARTESIAN_POINT ( 'NONE',  ( 8.731428362939190890, -13.89598863503036164, 27.21428571428572241 ) ) ;
#10001 = CYLINDRICAL_SURFACE ( 'NONE', #3190, 1.649999999999984812 ) ;
#10002 = CARTESIAN_POINT ( 'NONE',  ( -83.00000000000001421, 0.000000000000000000, 0.000000000000000000 ) ) ;
#10003 = CARTESIAN_POINT ( 'NONE',  ( 4.534861676072320158, -8.900167166472098046, 10.65000000000000924 ) ) ;
#10004 = CARTESIAN_POINT ( 'NONE',  ( -4.270415729527831772, -8.486213763410670907, 15.09886208192144430 ) ) ;
#10005 = CARTESIAN_POINT ( 'NONE',  ( -9.837026868206066865, 5.012215536711416064, 17.85000000000001918 ) ) ;
#10006 = CARTESIAN_POINT ( 'NONE',  ( -11.60466159355861926, -11.60466159355875249, 46.50000000000002132 ) ) ;
#10007 = CARTESIAN_POINT ( 'NONE',  ( 8.620103694221997515, 13.47998361472160767, 23.28975485534072121 ) ) ;
#10008 = CARTESIAN_POINT ( 'NONE',  ( -13.55419868402807992, -4.742819248065651472, 22.92857142857142705 ) ) ;
#10009 = CARTESIAN_POINT ( 'NONE',  ( 8.731428362939190890, -13.89598863503036164, 3.214285714285716633 ) ) ;
#10010 = CARTESIAN_POINT ( 'NONE',  ( -15.49051278174638036, -5.420364854932175902, 46.92857142857142350 ) ) ;
#10011 = ORIENTED_EDGE ( 'NONE', *, *, #2564, .F. ) ;
#10012 = CARTESIAN_POINT ( 'NONE',  ( -1.727091770866549414, -10.90442828429184630, 10.95000000000000462 ) ) ;
#10013 = DIRECTION ( 'NONE',  ( -1.000000000000000000, -1.387778780781445676E-16, -0.000000000000000000 ) ) ;
#10014 = CARTESIAN_POINT ( 'NONE',  ( 8.512513224245308763, 13.54758718765259040, 43.28571428571429180 ) ) ;
#10015 = CARTESIAN_POINT ( 'NONE',  ( -7.750357176954294935, 12.08964793087877787, 8.210245144659282346 ) ) ;
#10016 = CARTESIAN_POINT ( 'NONE',  ( 1.677562661911645714, 10.91227292449347175, 1.448862081921441947 ) ) ;
#10017 = CARTESIAN_POINT ( 'NONE',  ( -8.620103694221995738, -13.47998361472161299, 44.28975485534073186 ) ) ;
#10018 = APPLICATION_PROTOCOL_DEFINITION ( 'draft international standard', 'automotive_design', 1998, #4873 ) ;
#10019 = CARTESIAN_POINT ( 'NONE',  ( -12.15899005565164792, 7.639999817571650809, 29.78571428571428825 ) ) ;
#10020 = EDGE_CURVE ( 'NONE', #7029, #8895, #4808, .T. ) ;
#10021 = CARTESIAN_POINT ( 'NONE',  ( 13.17239914596754424, -4.743843029824685864, 24.57546914105500946 ) ) ;
#10022 = AXIS2_PLACEMENT_3D ( 'NONE', #1000, #2641, #850 ) ;
#10023 = EDGE_LOOP ( 'NONE', ( #3221, #2574, #65, #2478 ) ) ;
#10024 = CARTESIAN_POINT ( 'NONE',  ( -1.441234910513241818, -13.92619789766829008, 41.85310228751642825 ) ) ;
#10025 = EDGE_LOOP ( 'NONE', ( #4520, #204, #8813 ) ) ;
#10026 = DIRECTION ( 'NONE',  ( 1.000000000000000000, 0.000000000000000000, 0.000000000000000000 ) ) ;
#10027 = CARTESIAN_POINT ( 'NONE',  ( 5.404401153735178376, -15.06016580658422477, 29.42453085894499765 ) ) ;
#10028 = CARTESIAN_POINT ( 'NONE',  ( 13.89598863503045933, -8.731428362939032795, 8.785714285714290028 ) ) ;
#10029 = CARTESIAN_POINT ( 'NONE',  ( 7.027753727702739539, 7.098671581784288698, 1.748862081921432887 ) ) ;
#10030 = CARTESIAN_POINT ( 'NONE',  ( 13.51115193377584589, 4.865839792409294873, 45.92453085894500475 ) ) ;
#10031 = CARTESIAN_POINT ( 'NONE',  ( -9.814260835641038128, 5.056896391392221801, 13.85113791807855321 ) ) ;
#10032 = DIRECTION ( 'NONE',  ( 1.000000000000000000, 4.755747939841215952E-17, -0.000000000000000000 ) ) ;
#10033 = EDGE_CURVE ( 'NONE', #5107, #1541, #9628, .T. ) ;
#10034 = EDGE_LOOP ( 'NONE', ( #2946, #5873, #7582, #559 ) ) ;
#10035 = CARTESIAN_POINT ( 'NONE',  ( 8.404922754268618235, 13.61519076058357491, 51.28167371608785174 ) ) ;
#10036 = CARTESIAN_POINT ( 'NONE',  ( 1.727091770866551412, 10.90442828429187117, 0.4499999999999857447 ) ) ;
#10037 = CARTESIAN_POINT ( 'NONE',  ( -11.31370849898482156, 11.31370849898469544, 0.000000000000000000 ) ) ;
#10038 = CARTESIAN_POINT ( 'NONE',  ( -13.25633410266679313, 4.503970704919840529, 13.56738800180213822 ) ) ;
#10039 = CARTESIAN_POINT ( 'NONE',  ( 9.873755945037075321, 1.513077731353044131, 12.05113791807856671 ) ) ;
#10040 = CARTESIAN_POINT ( 'NONE',  ( 6.683790977649321619, -6.751237864895076157, 6.501137918078588207 ) ) ;
#10041 = CARTESIAN_POINT ( 'NONE',  ( -163.5777872869976761, -1.618470104113066910, 12.89924494662433396 ) ) ;
#10042 = CARTESIAN_POINT ( 'NONE',  ( -5.543385399275643444, -15.44746603149420494, 44.07546914105503078 ) ) ;
#10043 = CARTESIAN_POINT ( 'NONE',  ( -12.15899005565164792, 7.639999817571651697, 47.78571428571430602 ) ) ;
#10044 = CARTESIAN_POINT ( 'NONE',  ( -4.742819248065502258, -13.55419868402813677, 46.07142857142856940 ) ) ;
#10045 = EDGE_LOOP ( 'NONE', ( #6015, #8082, #3505, #8702, #1861, #6025, #3399, #1555, #407, #6049, #5728, #2423, #1877 ) ) ;
#10046 = CARTESIAN_POINT ( 'NONE',  ( 8.841785722321695573, -13.82664651025757152, 11.21024514465928235 ) ) ;
#10047 = DIRECTION ( 'NONE',  ( -1.000000000000000000, -0.000000000000000000, -0.000000000000000000 ) ) ;
#10048 = CARTESIAN_POINT ( 'NONE',  ( -13.89598863503046111, 8.731428362939027465, 35.78571428571429180 ) ) ;
#10049 = DIRECTION ( 'NONE',  ( 0.000000000000000000, 1.000000000000000000, 0.000000000000000000 ) ) ;
#10050 = DIRECTION ( 'NONE',  ( -1.000000000000000000, 1.842239752758738928E-31, -1.780435181894459419E-32 ) ) ;
#10051 = CARTESIAN_POINT ( 'NONE',  ( 7.806708723663831506, 7.806708723663930982, 0.7499999999999762412 ) ) ;
#10052 = CARTESIAN_POINT ( 'NONE',  ( -7.063212654743466601, -7.063212654743531438, 11.24999999999999467 ) ) ;
#10053 = CARTESIAN_POINT ( 'NONE',  ( 4.579542530753127672, -8.877401133907065756, 17.64886208192141126 ) ) ;
#10054 = CARTESIAN_POINT ( 'NONE',  ( 5.986002070941135678, -13.58603705635637304, 0.000000000000000000 ) ) ;
#10055 = ADVANCED_FACE ( 'NONE', ( #5529 ), #3209, .F. ) ;
#10056 = CARTESIAN_POINT ( 'NONE',  ( -11.22385875690717327, 11.40355824106234550, 22.00404056962643651 ) ) ;
#10057 = CARTESIAN_POINT ( 'NONE',  ( -5.284464991282755264, 15.10213328493384743, 48.42857142857143060 ) ) ;
#10058 = CARTESIAN_POINT ( 'NONE',  ( 16.29368510291089223, -1.967016585148476882, 18.36118342676929771 ) ) ;
#10059 = CARTESIAN_POINT ( 'NONE',  ( -13.54758718765249625, -8.512513224245459753, 22.71428571428571530 ) ) ;
#10060 = LINE ( 'NONE', #6676, #4634 ) ;
#10061 = VERTEX_POINT ( 'NONE', #7075 ) ;
#10062 = CARTESIAN_POINT ( 'NONE',  ( -1.642561882922479732, 10.37072757624895303, 18.29999999999998295 ) ) ;
#10063 = PRESENTATION_STYLE_ASSIGNMENT (( #6895 ) ) ;
#10064 = CARTESIAN_POINT ( 'NONE',  ( -15.10213328493390961, 5.284464991282586510, 41.57142857142856940 ) ) ;
#10065 = CARTESIAN_POINT ( 'NONE',  ( 4.724406229267374968, 9.377220287599055126, 4.598862081921435419 ) ) ;
#10066 = PRESENTATION_LAYER_ASSIGNMENT (  '', '', ( #3453 ) ) ;
#10067 = CARTESIAN_POINT ( 'NONE',  ( 8.621071003556677326, -13.96533075980314287, 43.21832628391217668 ) ) ;
#10068 = ITEM_DEFINED_TRANSFORMATION ( 'NONE', 'NONE', #7563,  #3995 ) ;
#10069 = CARTESIAN_POINT ( 'NONE',  ( 13.91197093850538380, 1.567502665446386390, 20.14285714285714235 ) ) ;
#10070 = CARTESIAN_POINT ( 'NONE',  ( 9.809645194534072132, -9.989344678689256796, 37.00404056962644006 ) ) ;
#10071 = CARTESIAN_POINT ( 'NONE',  ( -4.312909747525649706, -8.464561979789499091, 8.099999999999996092 ) ) ;
#10072 = CARTESIAN_POINT ( 'NONE',  ( 11.78653521626494793, 7.556039541191463371, 45.71024514465928235 ) ) ;
#10073 = AXIS2_PLACEMENT_3D ( 'NONE', #4607, #7758, #9475 ) ;
#10074 = EDGE_LOOP ( 'NONE', ( #8197, #8885 ) ) ;
#10075 = DIRECTION ( 'NONE',  ( 1.000000000000000000, 4.755747939841215952E-17, -0.000000000000000000 ) ) ;
#10076 = CARTESIAN_POINT ( 'NONE',  ( -15.88516839912898071, -1.917699372586004980, 25.13881657323070939 ) ) ;
#10077 = CIRCLE ( 'NONE', #7773, 13.00000000000000178 ) ;
#10078 = CARTESIAN_POINT ( 'NONE',  ( -2.000000000000002665, 18.00000000000000355, 0.000000000000000000 ) ) ;
#10079 = CARTESIAN_POINT ( 'NONE',  ( -9.858066664633883036, -1.612135949262833101, 12.54886208192144004 ) ) ;
#10080 = CARTESIAN_POINT ( 'NONE',  ( -8.841785722321695573, 13.82664651025757152, 26.21024514465928945 ) ) ;
#10081 = CARTESIAN_POINT ( 'NONE',  ( 9.837026868206066865, -5.012215536711392083, 7.350000000000000533 ) ) ;
#10082 = CARTESIAN_POINT ( 'NONE',  ( -10.91227292449344155, -1.677562661911749187, 13.55113791807856316 ) ) ;
#10083 = DIRECTION ( 'NONE',  ( 0.000000000000000000, 0.000000000000000000, -1.000000000000000000 ) ) ;
#10084 = CARTESIAN_POINT ( 'NONE',  ( -7.529642458189277576, 12.22833218042435455, 34.21832628391215536 ) ) ;
#10085 = AXIS2_PLACEMENT_3D ( 'NONE', #9999, #9803, #5849 ) ;
#10086 = AXIS2_PLACEMENT_3D ( 'NONE', #2784, #8271, #7546 ) ;
#10087 = FILL_AREA_STYLE_COLOUR ( '', #7554 ) ;
#10088 = EDGE_CURVE ( 'NONE', #2768, #9896, #7611, .T. ) ;
#10089 = CARTESIAN_POINT ( 'NONE',  ( 15.14410076328353227, -5.164528828830166063, 46.56738800180214355 ) ) ;
#10090 = CARTESIAN_POINT ( 'NONE',  ( 9.355568503977840678, 4.766900247265305701, 3.899999999999959055 ) ) ;
#10091 = CYLINDRICAL_SURFACE ( 'NONE', #1224, 13.00000000000001243 ) ;
#10092 = TOROIDAL_SURFACE ( 'NONE', #3153, 11.00000000000000355, 2.000000000000000000 ) ;
#10093 = AXIS2_PLACEMENT_3D ( 'NONE', #5445, #1529, #1627 ) ;
#10094 =( GEOMETRIC_REPRESENTATION_CONTEXT ( 3 ) GLOBAL_UNCERTAINTY_ASSIGNED_CONTEXT ( ( #2041 ) ) GLOBAL_UNIT_ASSIGNED_CONTEXT ( ( #9661, #8244, #9812 ) ) REPRESENTATION_CONTEXT ( 'NONE', 'WORKASPACE' ) );
#10095 = CARTESIAN_POINT ( 'NONE',  ( 11.78653521626494793, 7.556039541191463371, 21.71024514465928235 ) ) ;
#10096 = CARTESIAN_POINT ( 'NONE',  ( -1.612135949262737844, -9.858066664633888365, 15.95113791807857595 ) ) ;
#10097 = CARTESIAN_POINT ( 'NONE',  ( -7.098671581784199880, -7.027753727702804376, 1.251137918078559563 ) ) ;
#10098 = DIRECTION ( 'NONE',  ( 0.000000000000000000, 0.000000000000000000, -1.000000000000000000 ) ) ;
#10099 = CARTESIAN_POINT ( 'NONE',  ( -5.164528828830334817, 15.14410076328347543, 46.43261199819787066 ) ) ;
#10100 = CARTESIAN_POINT ( 'NONE',  ( -14.26974319298268767, 1.607813917172874918, 47.35714285714286120 ) ) ;
#10101 = CARTESIAN_POINT ( 'NONE',  ( -1.567502665446231180, -13.91197093850540334, 45.85714285714286120 ) ) ;
#10102 = EDGE_LOOP ( 'NONE', ( #821, #2443, #6437, #5702 ) ) ;
#10103 = CARTESIAN_POINT ( 'NONE',  ( -16.32287076676382398, 1.707986654103809343, 13.35310228751641937 ) ) ;
#10104 = CARTESIAN_POINT ( 'NONE',  ( 2.000000000000001776, 1.387778780781445676E-14, -1.535500000000022958 ) ) ;
#10105 = CARTESIAN_POINT ( 'NONE',  ( -13.89598863503046111, 8.731428362939027465, 23.78571428571429536 ) ) ;
#10106 = LINE ( 'NONE', #4625, #890 ) ;
#10107 = FACE_OUTER_BOUND ( 'NONE', #6473, .T. ) ;
#10108 = DIRECTION ( 'NONE',  ( 0.000000000000000000, -0.8660254037844391517, -0.4999999999999992228 ) ) ;
#10109 = CARTESIAN_POINT ( 'NONE',  ( 9.383039235653818366, -1.486127417882129986, 4.199999999999981526 ) ) ;
#10110 = CARTESIAN_POINT ( 'NONE',  ( -8.922933199037192509, 4.490180821391428267, 12.84886208192143009 ) ) ;
#10111 = DIRECTION ( 'NONE',  ( -4.755747939841215952E-17, 1.000000000000000000, 0.000000000000000000 ) ) ;
#10112 = CARTESIAN_POINT ( 'NONE',  ( -5.284464991282755264, 15.10213328493384743, 36.42857142857143060 ) ) ;
#10113 = CARTESIAN_POINT ( 'NONE',  ( 13.61519076058348254, 8.404922754268771001, 17.71832628391214826 ) ) ;
#10114 = CARTESIAN_POINT ( 'NONE',  ( 16.30827793483735633, -1.837501619626142890, 20.35714285714286476 ) ) ;
#10115 = LINE ( 'NONE', #5556, #4301 ) ;
#10116 = CARTESIAN_POINT ( 'NONE',  ( -1.642561882922479732, 10.37072757624895303, 15.29999999999997939 ) ) ;
#10117 = DIRECTION ( 'NONE',  ( -1.000000000000000000, 0.000000000000000000, 0.000000000000000000 ) ) ;
#10118 = CARTESIAN_POINT ( 'NONE',  ( -2.885895625854219215, 15.94142900571889143, 48.57768213684324365 ) ) ;
#10119 = CARTESIAN_POINT ( 'NONE',  ( -7.458344646081709328, 7.390897758835799358, 12.99886208192142512 ) ) ;
#10120 = CARTESIAN_POINT ( 'NONE',  ( 1.791431617652837316, 15.89939535829188877, 6.857142857142860315 ) ) ;
#10121 = CARTESIAN_POINT ( 'NONE',  ( 13.21436662431716869, -4.623906867372263640, 26.57142857142857295 ) ) ;
#10122 = CARTESIAN_POINT ( 'NONE',  ( 7.529642458189280241, -12.22833218042435099, 31.21832628391215536 ) ) ;
#10123 = CARTESIAN_POINT ( 'NONE',  ( -1.562606840307830591, -9.865911304835480067, 7.950000000000040146 ) ) ;
#10124 = ORIENTED_EDGE ( 'NONE', *, *, #6950, .F. ) ;
#10125 = CARTESIAN_POINT ( 'NONE',  ( -1.441234910513241818, -13.92619789766829008, 47.85310228751642114 ) ) ;
#10126 = ORIENTED_EDGE ( 'NONE', *, *, #5908, .F. ) ;
#10127 = DIRECTION ( 'NONE',  ( -1.000000000000000000, -0.000000000000000000, -0.000000000000000000 ) ) ;
#10128 = CARTESIAN_POINT ( 'NONE',  ( -8.841785722321695573, 13.82664651025757152, 26.21024514465928945 ) ) ;
#10129 = CARTESIAN_POINT ( 'NONE',  ( 11.60466159355861926, 11.60466159355874716, 7.500000000000004441 ) ) ;
#10130 = CARTESIAN_POINT ( 'NONE',  ( -4.270415729527831772, -8.486213763410678013, 12.09886208192144252 ) ) ;
#10131 = CARTESIAN_POINT ( 'NONE',  ( 11.40355824106246985, -11.22385875690704538, 28.99595943037357060 ) ) ;
#10132 = PLANE ( 'NONE',  #10073 ) ;
#10133 = CARTESIAN_POINT ( 'NONE',  ( -4.967534682030703586, 9.859792900771061852, 11.15113791807855215 ) ) ;
#10134 = CARTESIAN_POINT ( 'NONE',  ( 2.000000000000001776, 1.773042676681366281, 0.000000000000000000 ) ) ;
#10135 = CARTESIAN_POINT ( 'NONE',  ( -1.478298951650703019, 14.28433602490913579, 46.64689771248358596 ) ) ;
#10136 =( NAMED_UNIT ( * ) PLANE_ANGLE_UNIT ( ) SI_UNIT ( $, .RADIAN. ) );
#10137 = AXIS2_PLACEMENT_3D ( 'NONE', #4, #3006, #5334 ) ;
#10138 = CARTESIAN_POINT ( 'NONE',  ( -9.989344678689363377, 9.809645194533960222, 7.995959430373565269 ) ) ;
#10139 = CARTESIAN_POINT ( 'NONE',  ( -10.37072757624895836, 1.642561882922381145, 5.700000000000038369 ) ) ;
#10140 = CARTESIAN_POINT ( 'NONE',  ( 15.10213328493390783, -5.284464991282587398, 26.57142857142857295 ) ) ;
#10141 = CARTESIAN_POINT ( 'NONE',  ( -58.00000000000002842, 7.703719777548943412E-30, -1.059261469412979719E-30 ) ) ;
#10142 = CARTESIAN_POINT ( 'NONE',  ( -9.989344678689363377, 9.809645194533960222, 25.99595943037356349 ) ) ;
#10143 = CARTESIAN_POINT ( 'NONE',  ( 9.377220287599001836, 4.724406229267489543, 8.901137918078571687 ) ) ;
#10144 = EDGE_CURVE ( 'NONE', #2655, #2258, #9100, .T. ) ;
#10145 = CARTESIAN_POINT ( 'NONE',  ( -8.486213763410637156, -4.270415729527911708, 4.401137918078569022 ) ) ;
#10146 = CARTESIAN_POINT ( 'NONE',  ( -156.0000000000000284, -6.661338147750945553E-15, 0.000000000000000000 ) ) ;
#10147 = CARTESIAN_POINT ( 'NONE',  ( 8.621071003556677326, -13.96533075980314287, 43.21832628391217668 ) ) ;
#10148 = CARTESIAN_POINT ( 'NONE',  ( -13.92619789766827054, -1.441234910513399470, 9.146897712483580634 ) ) ;
#10149 = CARTESIAN_POINT ( 'NONE',  ( -1.607813917173034124, 14.26974319298267524, 48.64285714285716011 ) ) ;
#10150 = ORIENTED_EDGE ( 'NONE', *, *, #8566, .F. ) ;
#10151 = CARTESIAN_POINT ( 'NONE',  ( -1.967016585148659846, 16.29368510291087091, 14.63881657323070939 ) ) ;
#10152 = LINE ( 'NONE', #3065, #695 ) ;
#10153 = CARTESIAN_POINT ( 'NONE',  ( -15.89939535829186923, -1.791431617653016062, 41.14285714285714590 ) ) ;
#10154 = DIRECTION ( 'NONE',  ( 0.000000000000000000, -6.338944243255235518E-49, 1.000000000000000000 ) ) ;
#10155 = APPLICATION_CONTEXT ( 'automotive_design' ) ;
#10156 = CARTESIAN_POINT ( 'NONE',  ( 4.534861676072320158, -8.900167166472098046, 4.650000000000026112 ) ) ;
#10157 = CARTESIAN_POINT ( 'NONE',  ( -1.486127417882243895, 9.383039235653816590, 0.2999999999999669598 ) ) ;
#10158 = DIRECTION ( 'NONE',  ( 1.000000000000000000, 0.000000000000000000, 0.000000000000000000 ) ) ;
#10159 = CARTESIAN_POINT ( 'NONE',  ( 15.53355953199861794, 5.297344310588528060, 17.93261199819786711 ) ) ;
#10160 = CARTESIAN_POINT ( 'NONE',  ( 8.512513224245308763, 13.54758718765259040, 43.28571428571429180 ) ) ;
#10161 = CARTESIAN_POINT ( 'NONE',  ( -5.543385399275643444, -15.44746603149420494, 20.07546914105500591 ) ) ;
#10162 = CARTESIAN_POINT ( 'NONE',  ( -11.31370849898482156, 11.31370849898469544, 24.00000000000000000 ) ) ;
#10163 = DIRECTION ( 'NONE',  ( -1.000000000000000000, 4.575525868300071581E-16, 0.000000000000000000 ) ) ;
#10164 = PRODUCT_DEFINITION ( 'UNKNOWN', '', #4436, #1123 ) ;
#10165 = CARTESIAN_POINT ( 'NONE',  ( 11.31370849898482334, -11.31370849898469366, 9.000000000000001776 ) ) ;
#10166 = CARTESIAN_POINT ( 'NONE',  ( -5.420364854931998266, -15.49051278174643898, 40.07142857142857650 ) ) ;
#10167 = CARTESIAN_POINT ( 'NONE',  ( 4.724406229267374968, 9.377220287599055126, 13.59886208192140167 ) ) ;
#10168 = CARTESIAN_POINT ( 'NONE',  ( -1.791431617652833763, -15.89939535829188877, 3.857142857142857650 ) ) ;
#10169 = CARTESIAN_POINT ( 'NONE',  ( 1.837501619626330074, -16.30827793483733501, 3.642857142857144126 ) ) ;
#10170 = PRODUCT_CONTEXT ( 'NONE', #10155, 'mechanical' ) ;
#10171 = CARTESIAN_POINT ( 'NONE',  ( 13.91197093850538380, 1.567502665446386390, 44.14285714285714590 ) ) ;
#10172 = CARTESIAN_POINT ( 'NONE',  ( -11.92174236212692051, -7.340858601238089420, 38.71832628391214826 ) ) ;
#10173 = CARTESIAN_POINT ( 'NONE',  ( -4.534861676072319270, 8.900167166472124691, 9.150000000000002132 ) ) ;
#10174 = CARTESIAN_POINT ( 'NONE',  ( 9.837026868206066865, -5.012215536711395636, 16.35000000000000497 ) ) ;
#10175 = ORIENTED_EDGE ( 'NONE', *, *, #5440, .T. ) ;
#10176 = CARTESIAN_POINT ( 'NONE',  ( -11.78653521626494793, -7.556039541191465148, 42.71024514465928235 ) ) ;
#10177 = ORIENTED_EDGE ( 'NONE', *, *, #1371, .F. ) ;
#10178 = CARTESIAN_POINT ( 'NONE',  ( -5.110041130070070992, -16.97680807127747826, 0.000000000000000000 ) ) ;
#10179 = CARTESIAN_POINT ( 'NONE',  ( 5.404401153735178376, -15.06016580658422477, 17.42453085894499409 ) ) ;
#10180 = CARTESIAN_POINT ( 'NONE',  ( 5.284464991282756152, -15.10213328493384743, 9.428571428571425272 ) ) ;
#10181 = CARTESIAN_POINT ( 'NONE',  ( 8.442910196168311288, 4.355403765523574222, 10.89886208192140771 ) ) ;
#10182 = CARTESIAN_POINT ( 'NONE',  ( 8.841785722321695573, -13.82664651025757152, 23.21024514465928235 ) ) ;
#10183 = CARTESIAN_POINT ( 'NONE',  ( 0.000000000000000000, 0.000000000000000000, 0.000000000000000000 ) ) ;
#10184 = CARTESIAN_POINT ( 'NONE',  ( -9.355568503977838901, -4.766900247265280832, 8.399999999999963052 ) ) ;
#10185 = LINE ( 'NONE', #6192, #4145 ) ;
#10186 = CIRCLE ( 'NONE', #2095, 8.500000000000000000 ) ;
#10187 = EDGE_CURVE ( 'NONE', #6566, #6853, #1375, .T. ) ;
#10188 = ORIENTED_EDGE ( 'NONE', *, *, #3932, .T. ) ;
#10189 = CARTESIAN_POINT ( 'NONE',  ( 8.841785722321695573, -13.82664651025757152, 47.21024514465928235 ) ) ;
#10190 = VERTEX_POINT ( 'NONE', #3394 ) ;
#10191 = DIRECTION ( 'NONE',  ( 1.000000000000000000, 0.000000000000000000, 0.000000000000000000 ) ) ;
#10192 = CARTESIAN_POINT ( 'NONE',  ( -8.731428362939189114, 13.89598863503036341, 12.21428571428571885 ) ) ;
#10193 = FACE_OUTER_BOUND ( 'NONE', #8402, .T. ) ;
#10194 = CARTESIAN_POINT ( 'NONE',  ( -7.750357176954294935, 12.08964793087877787, 26.21024514465928945 ) ) ;
#10195 = CARTESIAN_POINT ( 'NONE',  ( 4.809394265263009061, 9.333916720356734587, 2.601137918078560762 ) ) ;
#10196 = CARTESIAN_POINT ( 'NONE',  ( -8.486213763410637156, -4.270415729527909043, 7.401137918078573463 ) ) ;
#10197 = DIRECTION ( 'NONE',  ( 0.000000000000000000, 8.191099868251448390E-34, 1.000000000000000000 ) ) ;
#10198 = CARTESIAN_POINT ( 'NONE',  ( -10.24623928997352351, -10.06191849875416899, 2.504040569626438728 ) ) ;
#10199 = CARTESIAN_POINT ( 'NONE',  ( 1.693770420379222319, 13.89774397934251837, 4.861183426769296823 ) ) ;
#10200 = ORIENTED_EDGE ( 'NONE', *, *, #5587, .F. ) ;
#10201 = CARTESIAN_POINT ( 'NONE',  ( 5.404401153735178376, -15.06016580658422477, 5.424530858944991429 ) ) ;
#10202 = CYLINDRICAL_SURFACE ( 'NONE', #4240, 3.500000000000000000 ) ;
#10203 = CARTESIAN_POINT ( 'NONE',  ( 8.731428362939190890, -13.89598863503036164, 45.21428571428572951 ) ) ;
#10204 = CARTESIAN_POINT ( 'NONE',  ( 2.000000000000001776, 1.773042676681366281, 0.000000000000000000 ) ) ;
#10205 = CARTESIAN_POINT ( 'NONE',  ( -9.511495879682431411E-16, 20.00000000000000000, 0.000000000000000000 ) ) ;
#10206 = CARTESIAN_POINT ( 'NONE',  ( 4.312909747525650594, 8.464561979789532842, 18.60000000000000497 ) ) ;
#10207 = CARTESIAN_POINT ( 'NONE',  ( 1.513077731352925115, 9.873755945037103743, 16.44886208192140131 ) ) ;
#10208 = EDGE_CURVE ( 'NONE', #3104, #7651, #4310, .T. ) ;
#10209 = CARTESIAN_POINT ( 'NONE',  ( -13.89598863503046111, 8.731428362939027465, 35.78571428571429180 ) ) ;
#10210 = LINE ( 'NONE', #6941, #5940 ) ;
#10211 = CARTESIAN_POINT ( 'NONE',  ( 13.82664651025767100, -8.841785722321541030, 30.78975485534071765 ) ) ;
#10212 = DIRECTION ( 'NONE',  ( -1.000000000000000000, -0.000000000000000000, -0.000000000000000000 ) ) ;
#10213 = CARTESIAN_POINT ( 'NONE',  ( 15.91362231745475597, 1.665163862720026255, 30.14689771248358241 ) ) ;
#10214 = ADVANCED_FACE ( 'NONE', ( #5151 ), #9707, .T. ) ;
#10215 = CARTESIAN_POINT ( 'NONE',  ( -11.31370849898482156, 11.31370849898469544, 11.99999999999999645 ) ) ;
#10216 = CARTESIAN_POINT ( 'NONE',  ( 10.73878802356280104, 11.43342105301867662, 48.73000000000003240 ) ) ;
#10217 = SHAPE_REPRESENTATION ( 'spring hault', ( #3995 ), #5470 ) ;
#10218 = CARTESIAN_POINT ( 'NONE',  ( 5.284464991282756152, -15.10213328493384743, 9.428571428571425272 ) ) ;
#10219 =( NAMED_UNIT ( * ) SI_UNIT ( $, .STERADIAN. ) SOLID_ANGLE_UNIT ( ) );
#10220 = CARTESIAN_POINT ( 'NONE',  ( -1.677562661911643938, -10.91227292449344688, 8.948862081921467038 ) ) ;
#10221 = CARTESIAN_POINT ( 'NONE',  ( -13.54758718765249625, -8.512513224245459753, 4.714285714285712636 ) ) ;
#10222 = CARTESIAN_POINT ( 'NONE',  ( -15.10213328493390961, 5.284464991282586510, 17.57142857142856940 ) ) ;
#10223 = ADVANCED_FACE ( 'NONE', ( #1898 ), #1842, .F. ) ;
#10224 = CARTESIAN_POINT ( 'NONE',  ( 1.607813917173037899, -14.26974319298267169, 33.64285714285714590 ) ) ;
#10225 = CARTESIAN_POINT ( 'NONE',  ( 14.25515036105622535, -1.737328882695210241, 36.36118342676930126 ) ) ;
#10226 = CARTESIAN_POINT ( 'NONE',  ( 8.900167166472158442, -4.534861676072210912, 13.34999999999998543 ) ) ;
#10227 = ORIENTED_EDGE ( 'NONE', *, *, #7151, .T. ) ;
#10228 = NEXT_ASSEMBLY_USAGE_OCCURRENCE ( 'NAUO1', ' ', ' ', #6036, #4671, $ ) ;
#10229 = NEXT_ASSEMBLY_USAGE_OCCURRENCE ( 'NAUO2', ' ', ' ', #6036, #5604, $ ) ;
#10230 = NEXT_ASSEMBLY_USAGE_OCCURRENCE ( 'NAUO3', ' ', ' ', #6036, #4346, $ ) ;
#10231 = NEXT_ASSEMBLY_USAGE_OCCURRENCE ( 'NAUO4', ' ', ' ', #6036, #7569, $ ) ;
#10232 = NEXT_ASSEMBLY_USAGE_OCCURRENCE ( 'NAUO5', ' ', ' ', #6036, #6660, $ ) ;
#10233 = NEXT_ASSEMBLY_USAGE_OCCURRENCE ( 'NAUO6', ' ', ' ', #6036, #6660, $ ) ;
#10234 = NEXT_ASSEMBLY_USAGE_OCCURRENCE ( 'NAUO7', ' ', ' ', #6036, #7252, $ ) ;
#10235 = NEXT_ASSEMBLY_USAGE_OCCURRENCE ( 'NAUO8', ' ', ' ', #6036, #9415, $ ) ;
#10236 = NEXT_ASSEMBLY_USAGE_OCCURRENCE ( 'NAUO9', ' ', ' ', #6036, #8652, $ ) ;
#10237 = NEXT_ASSEMBLY_USAGE_OCCURRENCE ( 'NAUO10', ' ', ' ', #6036, #10164, $ ) ;
#10238 = NEXT_ASSEMBLY_USAGE_OCCURRENCE ( 'NAUO11', ' ', ' ', #6036, #8011, $ ) ;
#10239 = NEXT_ASSEMBLY_USAGE_OCCURRENCE ( 'NAUO12', ' ', ' ', #6036, #9288, $ ) ;
ENDSEC;
END-ISO-10303-21;
